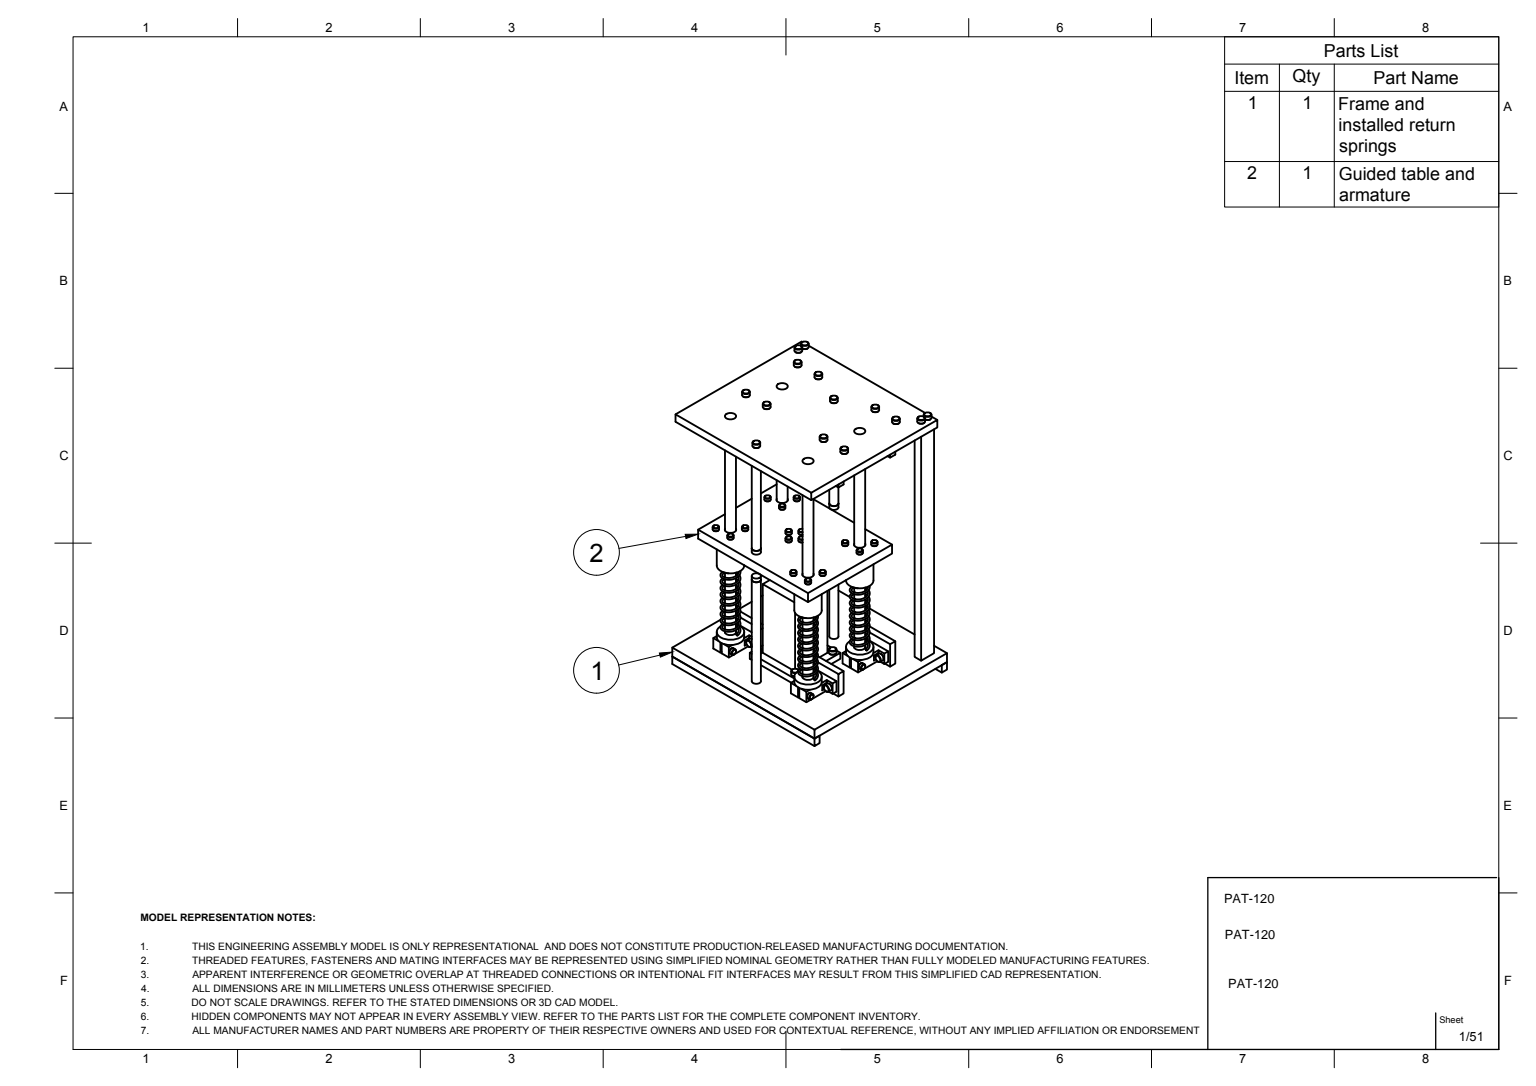
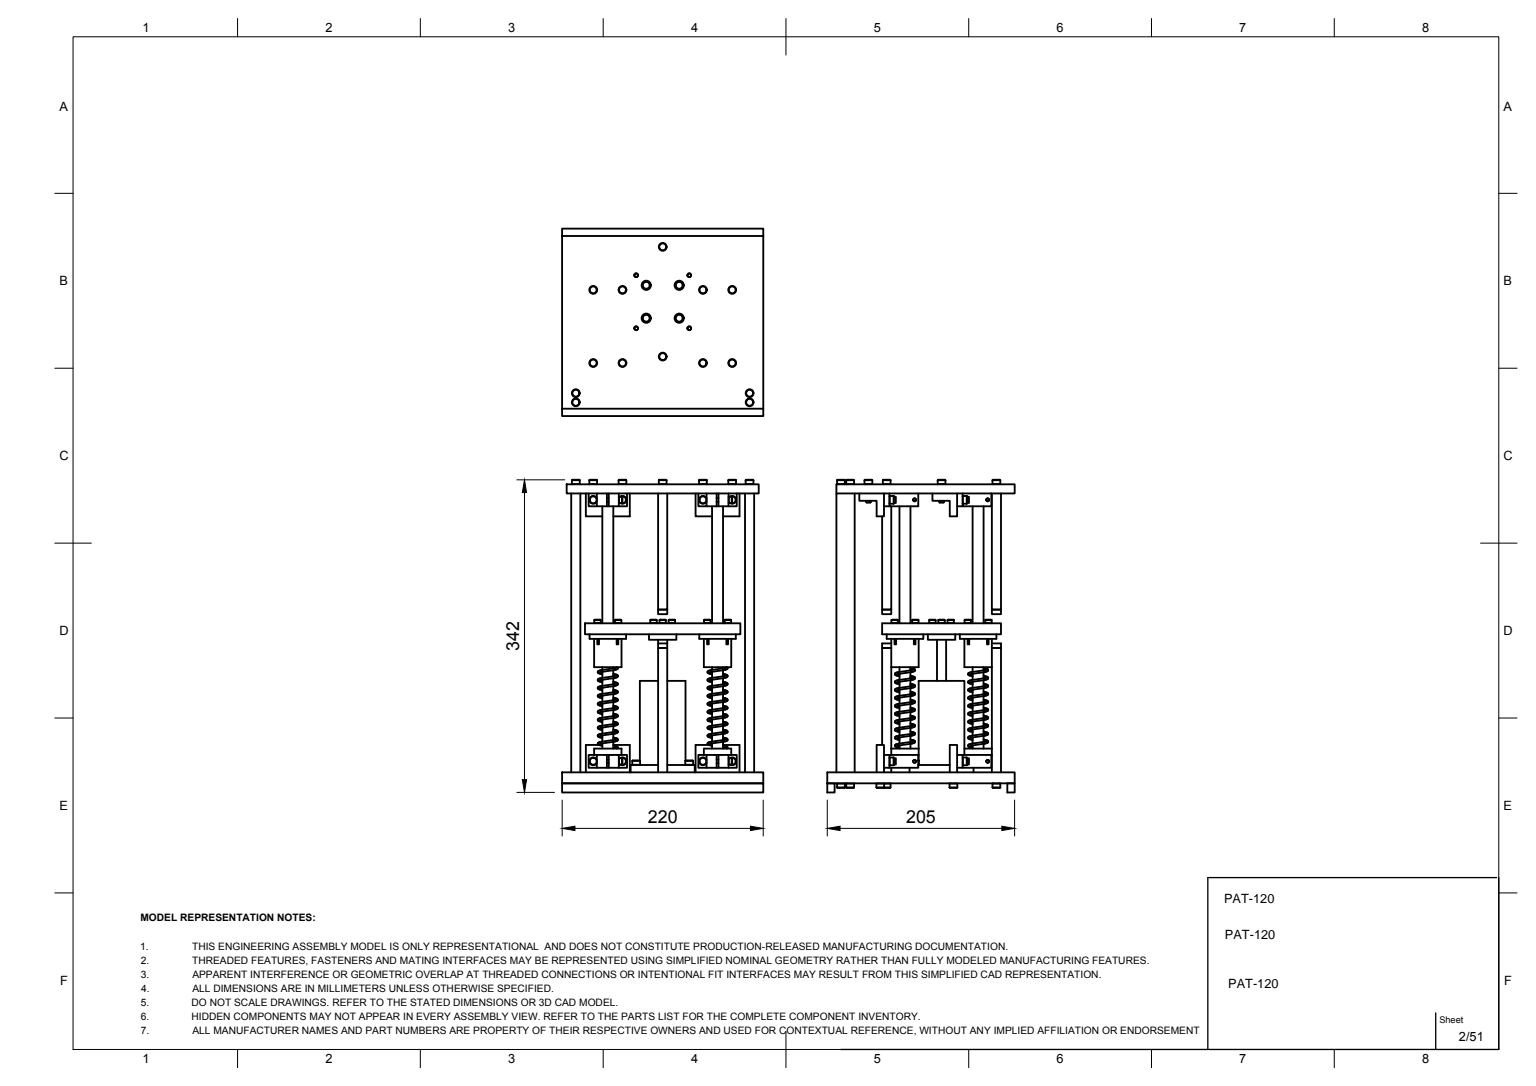
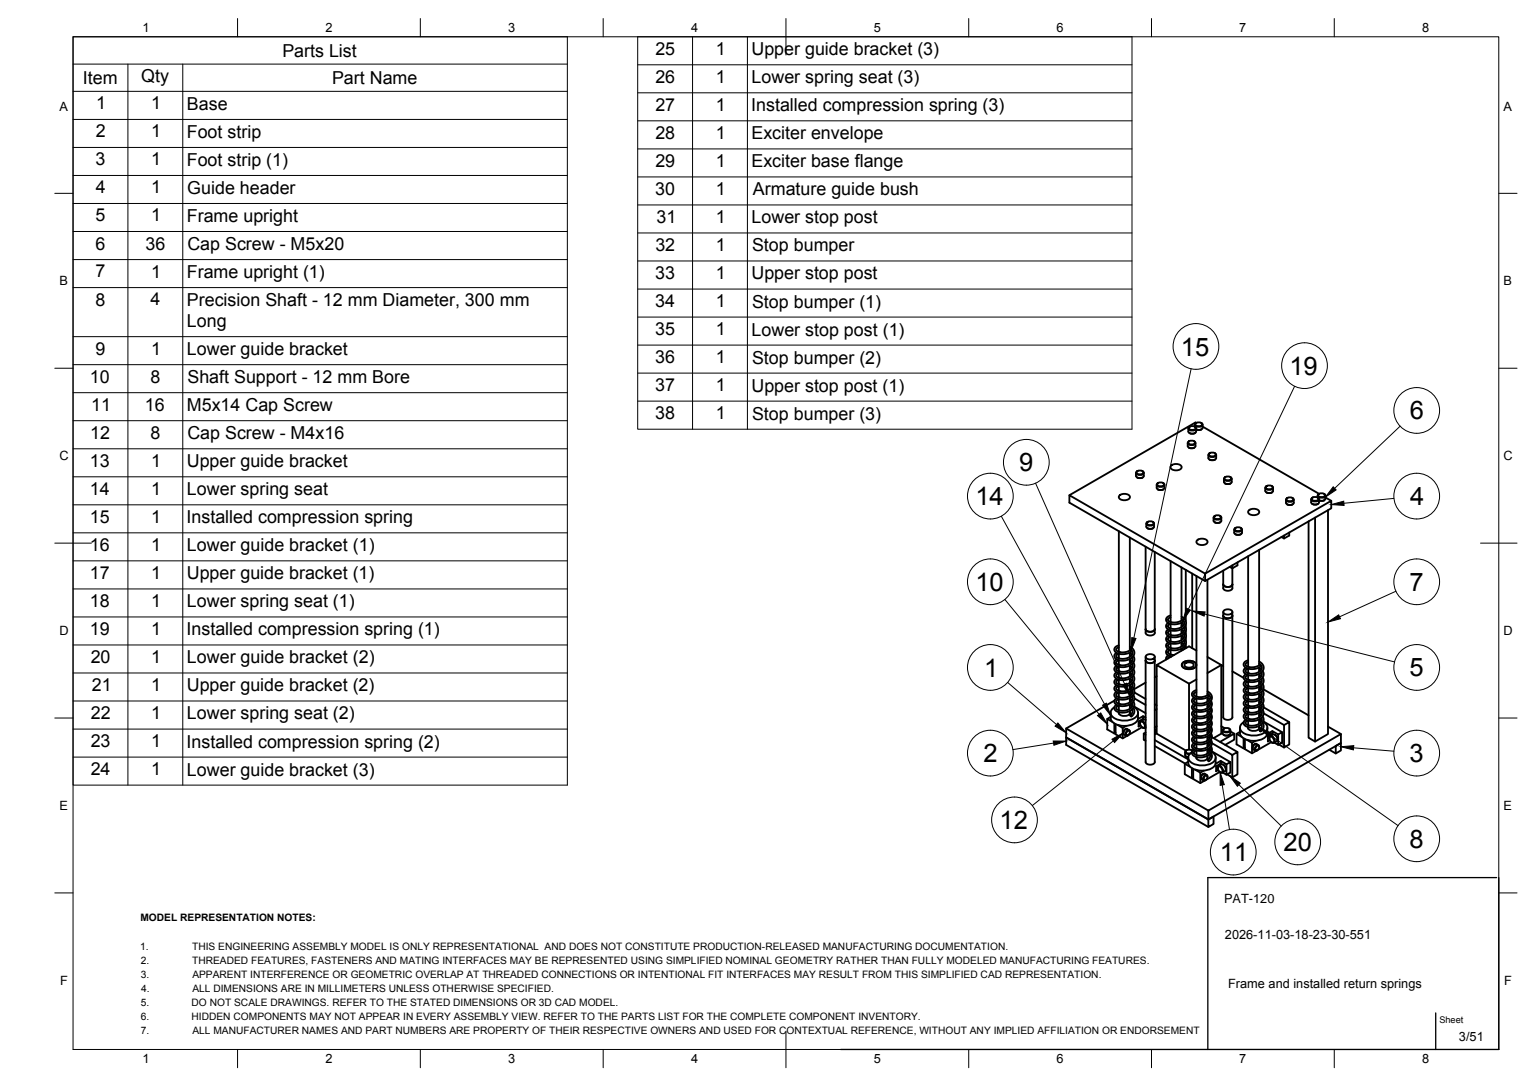
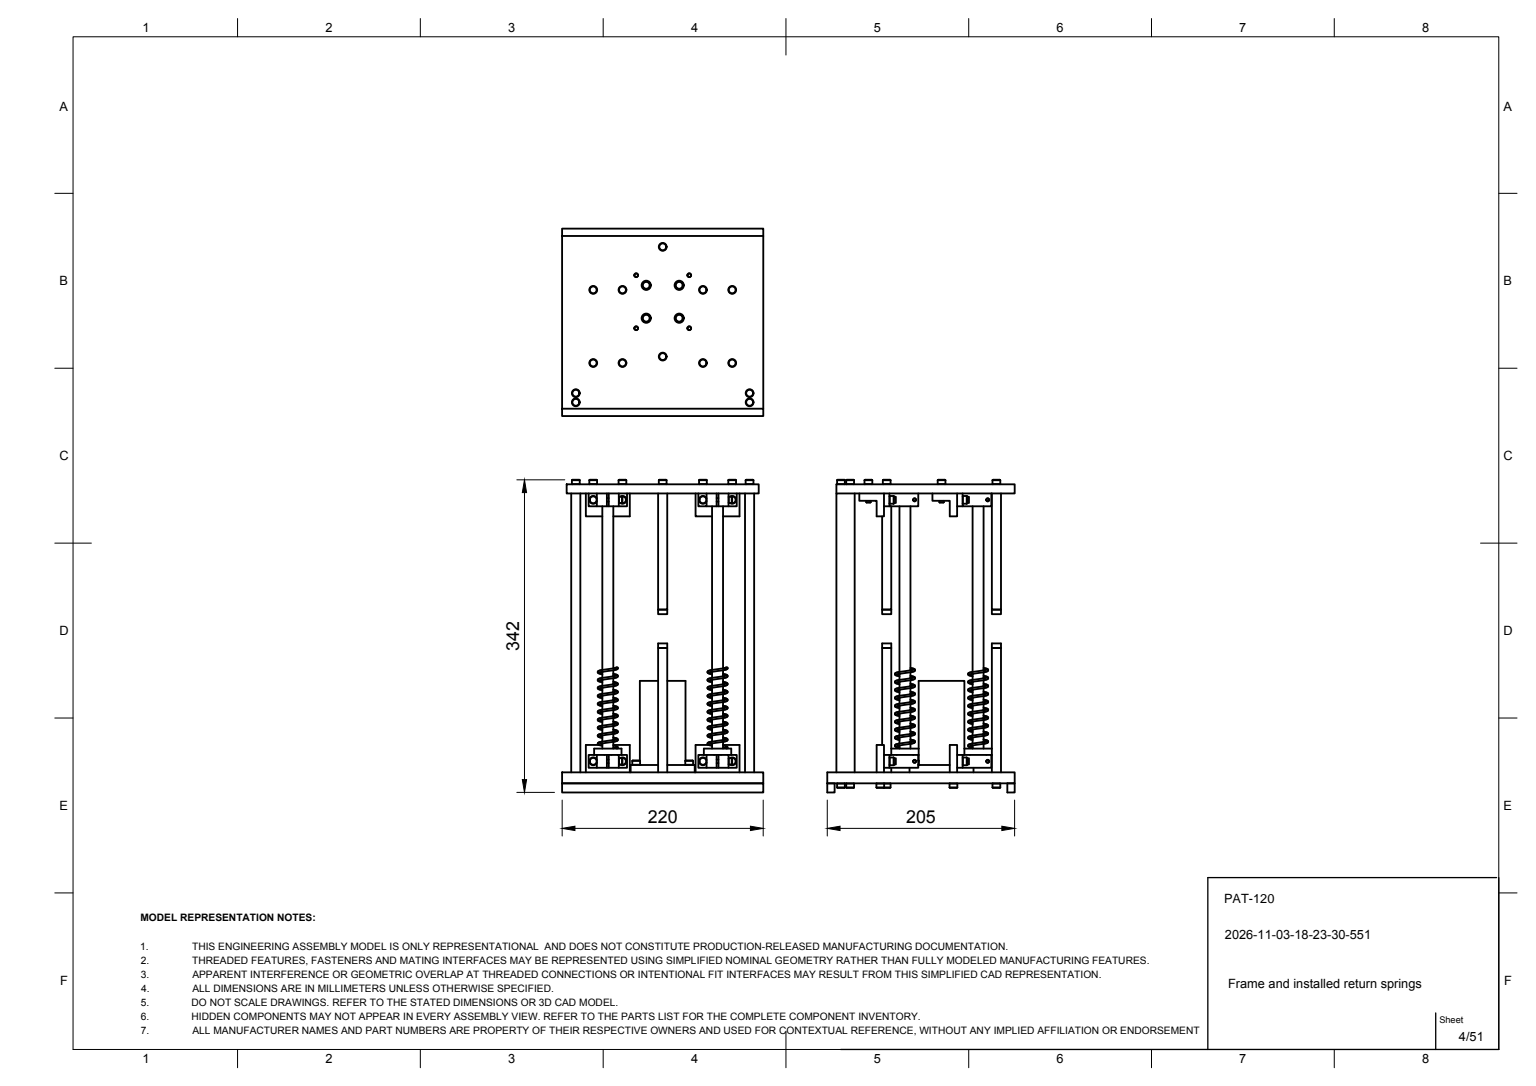
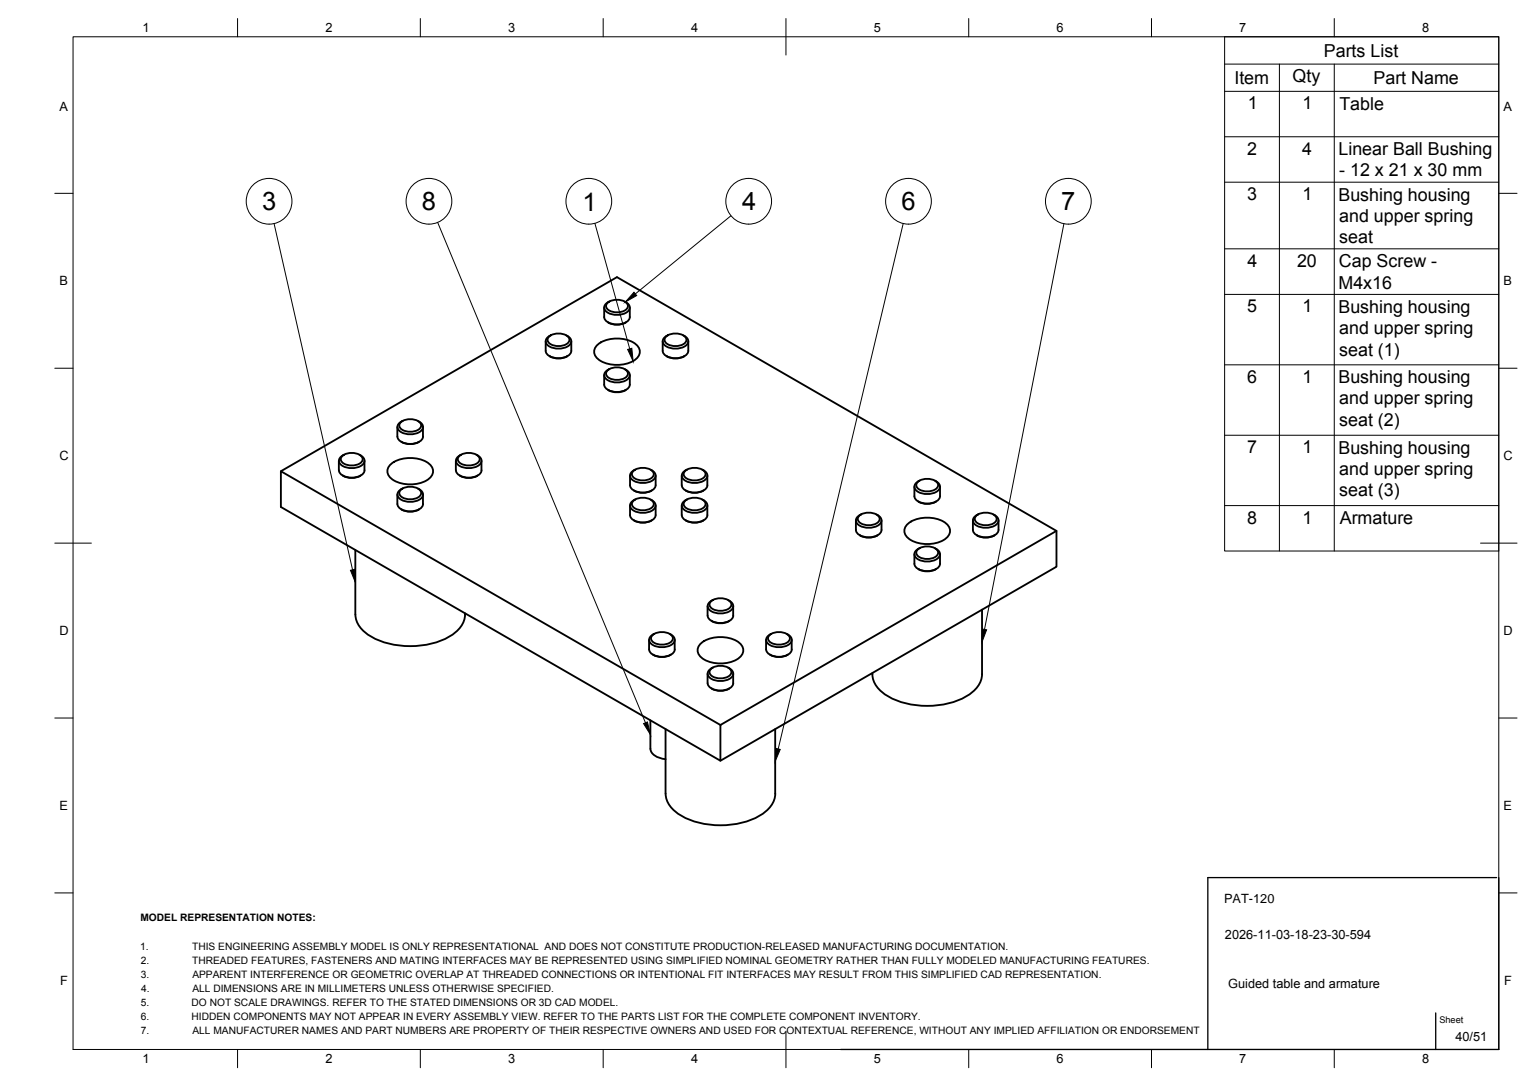
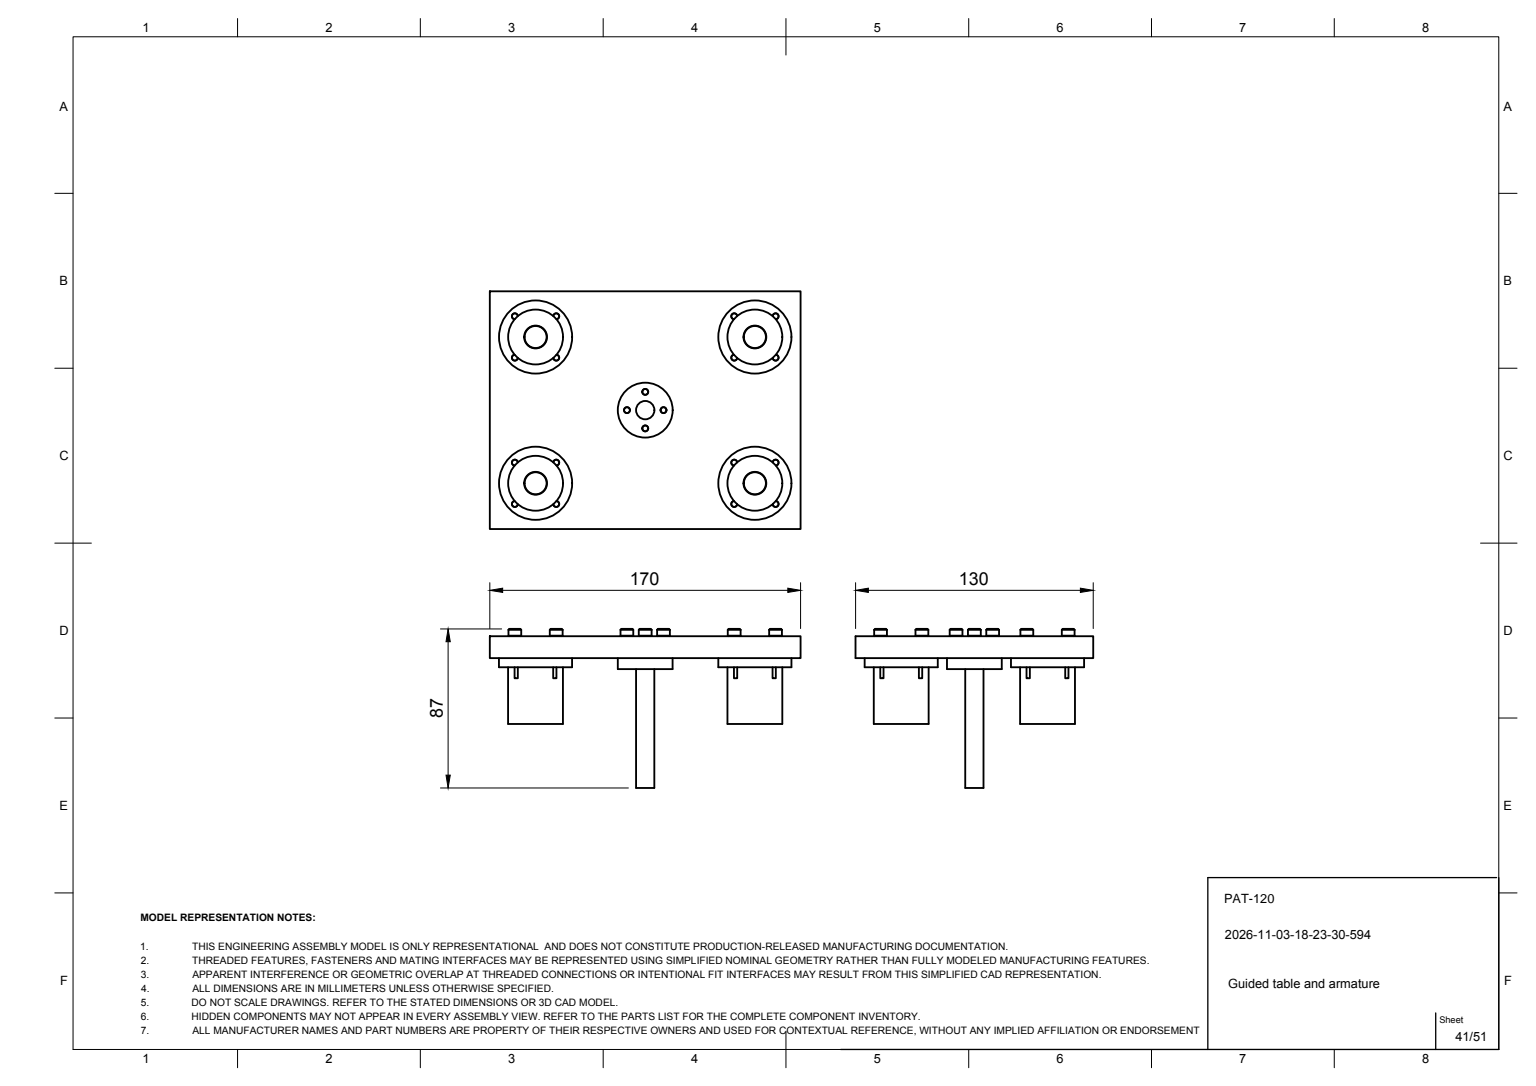
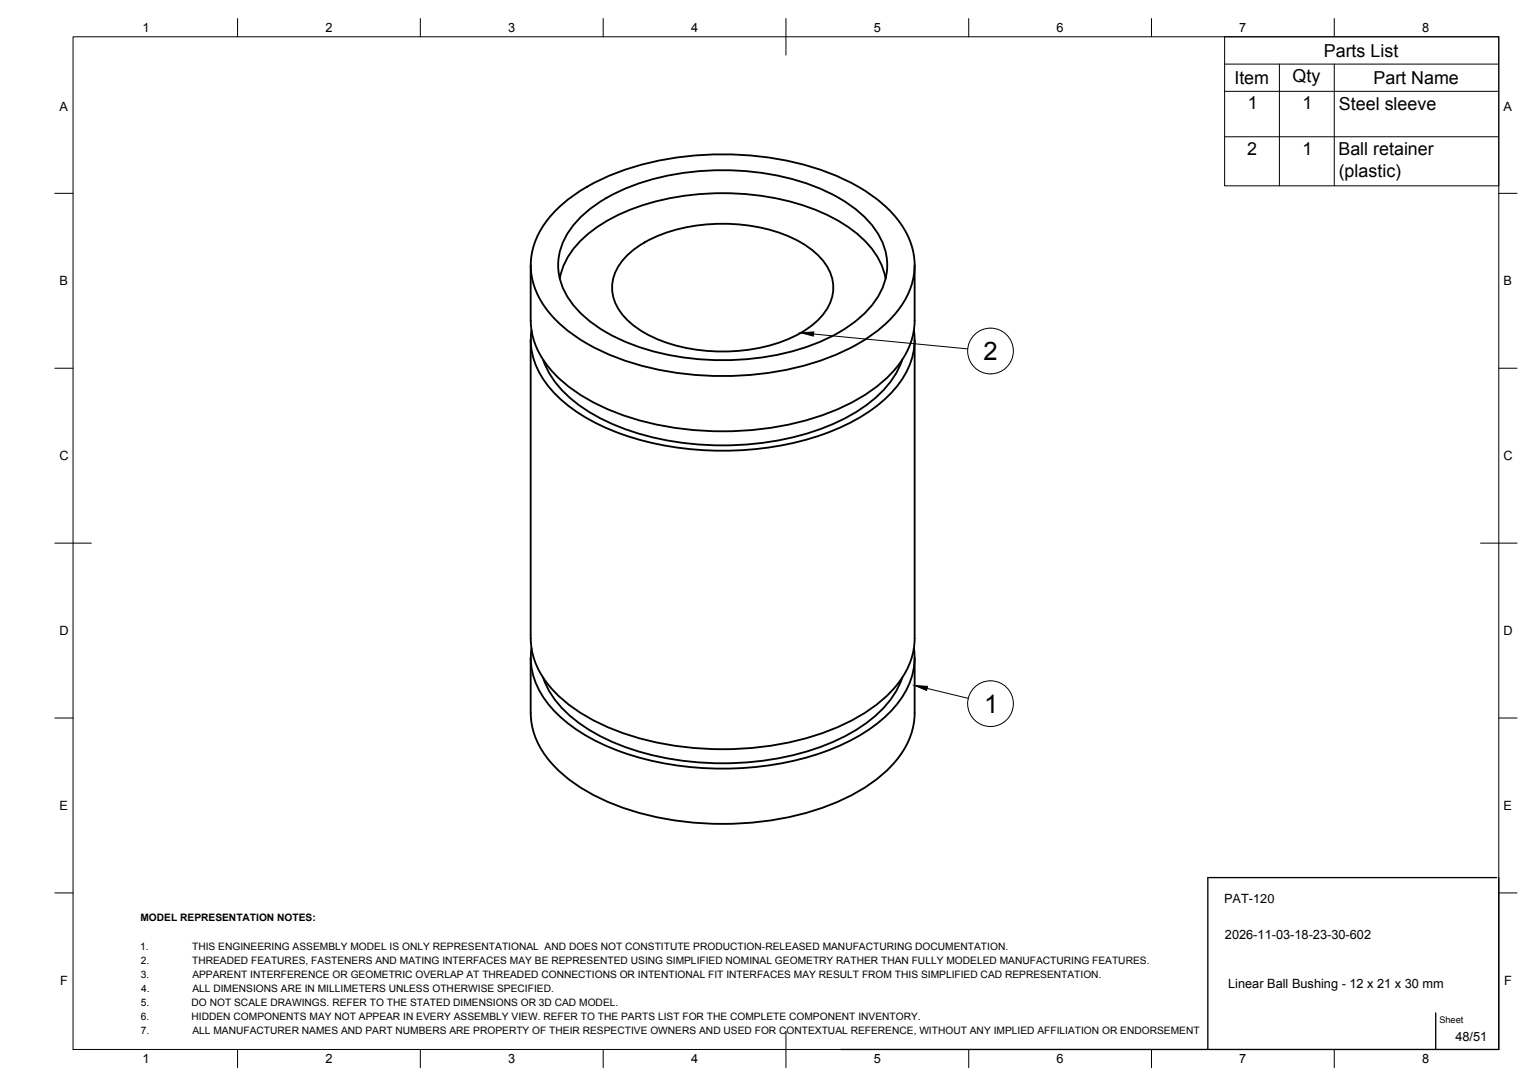
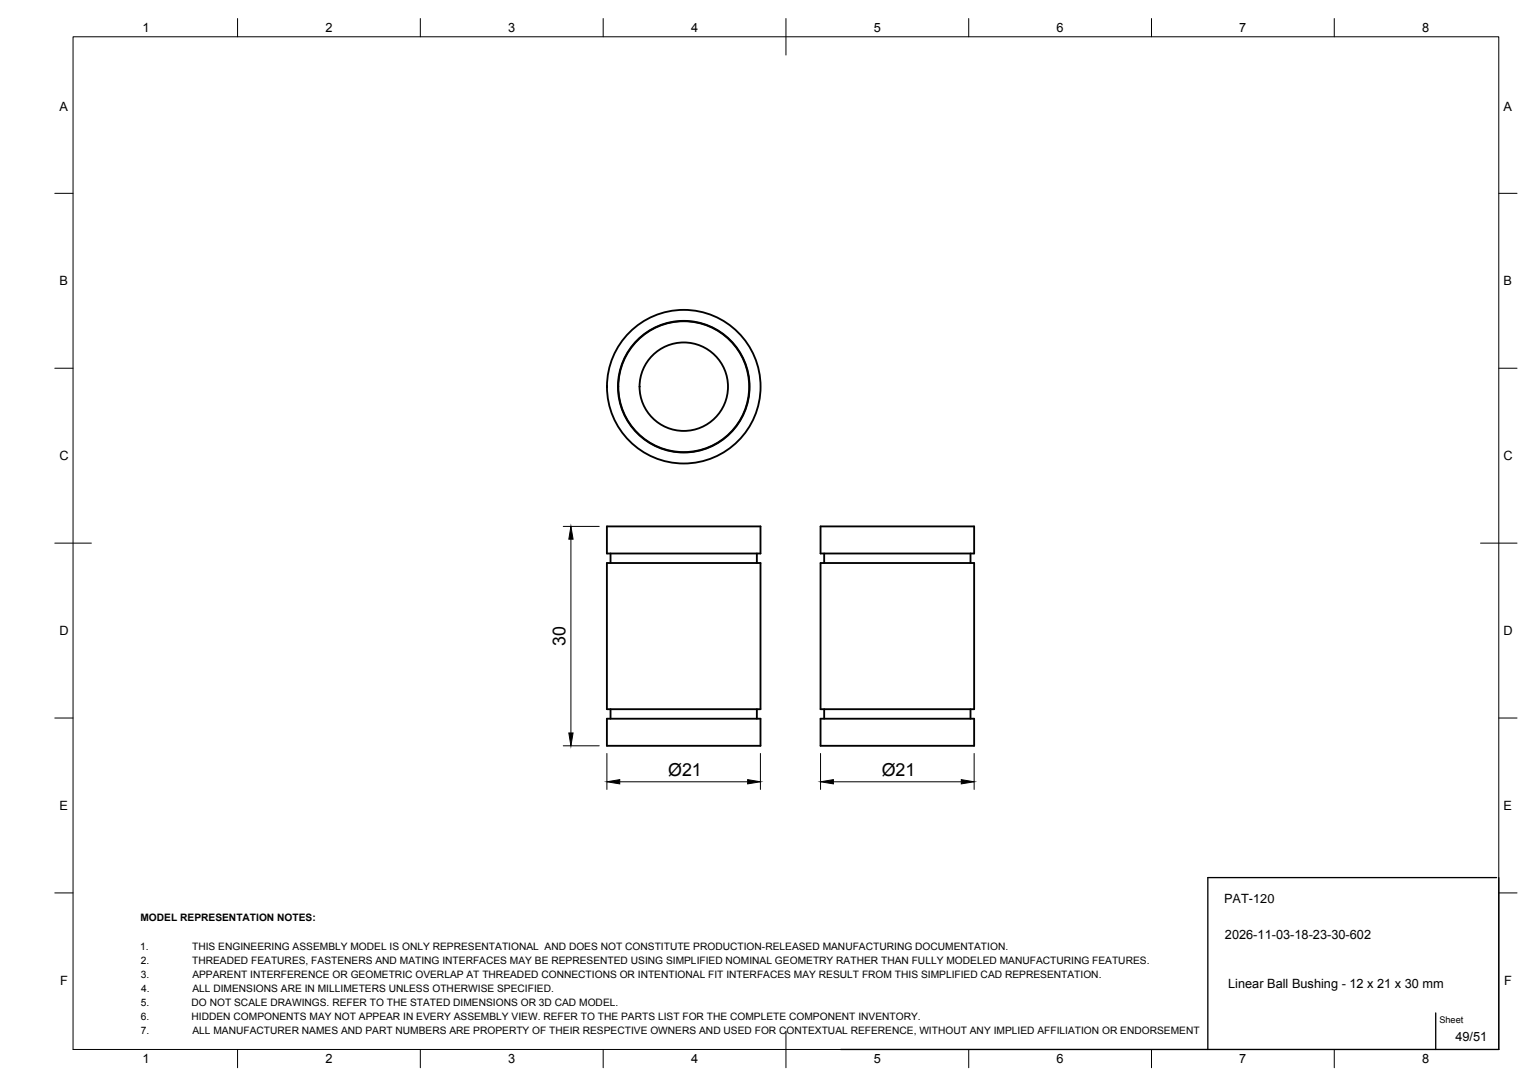
ISO-10303-21;
HEADER;
/* Generated by software containing ST-Developer
 * from STEP Tools, Inc. (www.steptools.com) 
 */

FILE_DESCRIPTION(
/* description */ ('Vibration shaker table dummy'),
/* implementation_level */ '2;1');

FILE_NAME(
/* name */ 'PAT-120',
/* time_stamp */ '2026-10-27T10:55:14-07:00',
/* author */ (''),
/* organization */ (''),
/* preprocessor_version */ 'ST-DEVELOPER v20.2',
/* originating_system */ 'Autodesk Translation Framework v15.17.0.0',
/* authorisation */ '');

FILE_SCHEMA (('AUTOMOTIVE_DESIGN { 1 0 10303 214 3 1 1 }'));
ENDSEC;

DATA;
#10=MECHANICAL_DESIGN_GEOMETRIC_PRESENTATION_REPRESENTATION('',(#686,#687,
#688,#689,#690,#691,#692,#693,#694,#695,#696,#697,#698,#699,#700,#701,#702,
#703,#704,#705,#706,#707,#708,#709,#710,#711,#712,#713,#714,#715,#716,#717,
#718,#719,#720,#721,#722,#723,#724,#725,#726,#727,#728,#729,#730,#731),
#22394);
#11=ITEM_DEFINED_TRANSFORMATION($,$,#10736,#10785);
#12=ITEM_DEFINED_TRANSFORMATION($,$,#10768,#10786);
#13=ITEM_DEFINED_TRANSFORMATION($,$,#9762,#10813);
#14=ITEM_DEFINED_TRANSFORMATION($,$,#9835,#10814);
#15=ITEM_DEFINED_TRANSFORMATION($,$,#9842,#10815);
#16=ITEM_DEFINED_TRANSFORMATION($,$,#9849,#10816);
#17=ITEM_DEFINED_TRANSFORMATION($,$,#9910,#10817);
#18=ITEM_DEFINED_TRANSFORMATION($,$,#9933,#10818);
#19=ITEM_DEFINED_TRANSFORMATION($,$,#9956,#10819);
#20=ITEM_DEFINED_TRANSFORMATION($,$,#9977,#10820);
#21=ITEM_DEFINED_TRANSFORMATION($,$,#10004,#10821);
#22=ITEM_DEFINED_TRANSFORMATION($,$,#10013,#10822);
#23=ITEM_DEFINED_TRANSFORMATION($,$,#10018,#10823);
#24=ITEM_DEFINED_TRANSFORMATION($,$,#10039,#10824);
#25=ITEM_DEFINED_TRANSFORMATION($,$,#10066,#10825);
#26=ITEM_DEFINED_TRANSFORMATION($,$,#10075,#10826);
#27=ITEM_DEFINED_TRANSFORMATION($,$,#10080,#10827);
#28=ITEM_DEFINED_TRANSFORMATION($,$,#10101,#10828);
#29=ITEM_DEFINED_TRANSFORMATION($,$,#10128,#10829);
#30=ITEM_DEFINED_TRANSFORMATION($,$,#10137,#10830);
#31=ITEM_DEFINED_TRANSFORMATION($,$,#10142,#10831);
#32=ITEM_DEFINED_TRANSFORMATION($,$,#10163,#10832);
#33=ITEM_DEFINED_TRANSFORMATION($,$,#10190,#10833);
#34=ITEM_DEFINED_TRANSFORMATION($,$,#10199,#10834);
#35=ITEM_DEFINED_TRANSFORMATION($,$,#10204,#10835);
#36=ITEM_DEFINED_TRANSFORMATION($,$,#10235,#10836);
#37=ITEM_DEFINED_TRANSFORMATION($,$,#10266,#10837);
#38=ITEM_DEFINED_TRANSFORMATION($,$,#10275,#10838);
#39=ITEM_DEFINED_TRANSFORMATION($,$,#10285,#10839);
#40=ITEM_DEFINED_TRANSFORMATION($,$,#10291,#10840);
#41=ITEM_DEFINED_TRANSFORMATION($,$,#10301,#10841);
#42=ITEM_DEFINED_TRANSFORMATION($,$,#10307,#10842);
#43=ITEM_DEFINED_TRANSFORMATION($,$,#10317,#10843);
#44=ITEM_DEFINED_TRANSFORMATION($,$,#10323,#10844);
#45=ITEM_DEFINED_TRANSFORMATION($,$,#10333,#10845);
#46=ITEM_DEFINED_TRANSFORMATION($,$,#10411,#10846);
#47=ITEM_DEFINED_TRANSFORMATION($,$,#10411,#10847);
#48=ITEM_DEFINED_TRANSFORMATION($,$,#10411,#10848);
#49=ITEM_DEFINED_TRANSFORMATION($,$,#10411,#10849);
#50=ITEM_DEFINED_TRANSFORMATION($,$,#10411,#10850);
#51=ITEM_DEFINED_TRANSFORMATION($,$,#10411,#10851);
#52=ITEM_DEFINED_TRANSFORMATION($,$,#10411,#10852);
#53=ITEM_DEFINED_TRANSFORMATION($,$,#10411,#10853);
#54=ITEM_DEFINED_TRANSFORMATION($,$,#10339,#10854);
#55=ITEM_DEFINED_TRANSFORMATION($,$,#10349,#10855);
#56=ITEM_DEFINED_TRANSFORMATION($,$,#10387,#10856);
#57=ITEM_DEFINED_TRANSFORMATION($,$,#10387,#10857);
#58=ITEM_DEFINED_TRANSFORMATION($,$,#10787,#10858);
#59=ITEM_DEFINED_TRANSFORMATION($,$,#10411,#10859);
#60=ITEM_DEFINED_TRANSFORMATION($,$,#10411,#10860);
#61=ITEM_DEFINED_TRANSFORMATION($,$,#10349,#10861);
#62=ITEM_DEFINED_TRANSFORMATION($,$,#10387,#10862);
#63=ITEM_DEFINED_TRANSFORMATION($,$,#10387,#10863);
#64=ITEM_DEFINED_TRANSFORMATION($,$,#10787,#10864);
#65=ITEM_DEFINED_TRANSFORMATION($,$,#10411,#10865);
#66=ITEM_DEFINED_TRANSFORMATION($,$,#10411,#10866);
#67=ITEM_DEFINED_TRANSFORMATION($,$,#10339,#10867);
#68=ITEM_DEFINED_TRANSFORMATION($,$,#10349,#10868);
#69=ITEM_DEFINED_TRANSFORMATION($,$,#10387,#10869);
#70=ITEM_DEFINED_TRANSFORMATION($,$,#10387,#10870);
#71=ITEM_DEFINED_TRANSFORMATION($,$,#10787,#10871);
#72=ITEM_DEFINED_TRANSFORMATION($,$,#10411,#10872);
#73=ITEM_DEFINED_TRANSFORMATION($,$,#10411,#10873);
#74=ITEM_DEFINED_TRANSFORMATION($,$,#10349,#10874);
#75=ITEM_DEFINED_TRANSFORMATION($,$,#10387,#10875);
#76=ITEM_DEFINED_TRANSFORMATION($,$,#10387,#10876);
#77=ITEM_DEFINED_TRANSFORMATION($,$,#10787,#10877);
#78=ITEM_DEFINED_TRANSFORMATION($,$,#10411,#10878);
#79=ITEM_DEFINED_TRANSFORMATION($,$,#10411,#10879);
#80=ITEM_DEFINED_TRANSFORMATION($,$,#10339,#10880);
#81=ITEM_DEFINED_TRANSFORMATION($,$,#10349,#10881);
#82=ITEM_DEFINED_TRANSFORMATION($,$,#10387,#10882);
#83=ITEM_DEFINED_TRANSFORMATION($,$,#10387,#10883);
#84=ITEM_DEFINED_TRANSFORMATION($,$,#10787,#10884);
#85=ITEM_DEFINED_TRANSFORMATION($,$,#10411,#10885);
#86=ITEM_DEFINED_TRANSFORMATION($,$,#10411,#10886);
#87=ITEM_DEFINED_TRANSFORMATION($,$,#10349,#10887);
#88=ITEM_DEFINED_TRANSFORMATION($,$,#10387,#10888);
#89=ITEM_DEFINED_TRANSFORMATION($,$,#10387,#10889);
#90=ITEM_DEFINED_TRANSFORMATION($,$,#10787,#10890);
#91=ITEM_DEFINED_TRANSFORMATION($,$,#10411,#10891);
#92=ITEM_DEFINED_TRANSFORMATION($,$,#10411,#10892);
#93=ITEM_DEFINED_TRANSFORMATION($,$,#10339,#10893);
#94=ITEM_DEFINED_TRANSFORMATION($,$,#10349,#10894);
#95=ITEM_DEFINED_TRANSFORMATION($,$,#10387,#10895);
#96=ITEM_DEFINED_TRANSFORMATION($,$,#10387,#10896);
#97=ITEM_DEFINED_TRANSFORMATION($,$,#10787,#10897);
#98=ITEM_DEFINED_TRANSFORMATION($,$,#10411,#10898);
#99=ITEM_DEFINED_TRANSFORMATION($,$,#10411,#10899);
#100=ITEM_DEFINED_TRANSFORMATION($,$,#10349,#10900);
#101=ITEM_DEFINED_TRANSFORMATION($,$,#10387,#10901);
#102=ITEM_DEFINED_TRANSFORMATION($,$,#10387,#10902);
#103=ITEM_DEFINED_TRANSFORMATION($,$,#10787,#10903);
#104=ITEM_DEFINED_TRANSFORMATION($,$,#10411,#10904);
#105=ITEM_DEFINED_TRANSFORMATION($,$,#10411,#10905);
#106=ITEM_DEFINED_TRANSFORMATION($,$,#10411,#10906);
#107=ITEM_DEFINED_TRANSFORMATION($,$,#10411,#10907);
#108=ITEM_DEFINED_TRANSFORMATION($,$,#10411,#10908);
#109=ITEM_DEFINED_TRANSFORMATION($,$,#10411,#10909);
#110=ITEM_DEFINED_TRANSFORMATION($,$,#10411,#10910);
#111=ITEM_DEFINED_TRANSFORMATION($,$,#10411,#10911);
#112=ITEM_DEFINED_TRANSFORMATION($,$,#10411,#10912);
#113=ITEM_DEFINED_TRANSFORMATION($,$,#10411,#10913);
#114=ITEM_DEFINED_TRANSFORMATION($,$,#10411,#10914);
#115=ITEM_DEFINED_TRANSFORMATION($,$,#10411,#10915);
#116=ITEM_DEFINED_TRANSFORMATION($,$,#10411,#10916);
#117=ITEM_DEFINED_TRANSFORMATION($,$,#10411,#10917);
#118=ITEM_DEFINED_TRANSFORMATION($,$,#10438,#10918);
#119=ITEM_DEFINED_TRANSFORMATION($,$,#10517,#10919);
#120=ITEM_DEFINED_TRANSFORMATION($,$,#10566,#10920);
#121=ITEM_DEFINED_TRANSFORMATION($,$,#10615,#10921);
#122=ITEM_DEFINED_TRANSFORMATION($,$,#10664,#10922);
#123=ITEM_DEFINED_TRANSFORMATION($,$,#10713,#10923);
#124=ITEM_DEFINED_TRANSFORMATION($,$,#10735,#10924);
#125=ITEM_DEFINED_TRANSFORMATION($,$,#10787,#10925);
#126=ITEM_DEFINED_TRANSFORMATION($,$,#10787,#10926);
#127=ITEM_DEFINED_TRANSFORMATION($,$,#10787,#10927);
#128=ITEM_DEFINED_TRANSFORMATION($,$,#10787,#10928);
#129=ITEM_DEFINED_TRANSFORMATION($,$,#10735,#10929);
#130=ITEM_DEFINED_TRANSFORMATION($,$,#10787,#10930);
#131=ITEM_DEFINED_TRANSFORMATION($,$,#10787,#10931);
#132=ITEM_DEFINED_TRANSFORMATION($,$,#10787,#10932);
#133=ITEM_DEFINED_TRANSFORMATION($,$,#10787,#10933);
#134=ITEM_DEFINED_TRANSFORMATION($,$,#10735,#10934);
#135=ITEM_DEFINED_TRANSFORMATION($,$,#10787,#10935);
#136=ITEM_DEFINED_TRANSFORMATION($,$,#10787,#10936);
#137=ITEM_DEFINED_TRANSFORMATION($,$,#10787,#10937);
#138=ITEM_DEFINED_TRANSFORMATION($,$,#10787,#10938);
#139=ITEM_DEFINED_TRANSFORMATION($,$,#10735,#10939);
#140=ITEM_DEFINED_TRANSFORMATION($,$,#10787,#10940);
#141=ITEM_DEFINED_TRANSFORMATION($,$,#10787,#10941);
#142=ITEM_DEFINED_TRANSFORMATION($,$,#10787,#10942);
#143=ITEM_DEFINED_TRANSFORMATION($,$,#10787,#10943);
#144=ITEM_DEFINED_TRANSFORMATION($,$,#10787,#10944);
#145=ITEM_DEFINED_TRANSFORMATION($,$,#10787,#10945);
#146=ITEM_DEFINED_TRANSFORMATION($,$,#10787,#10946);
#147=ITEM_DEFINED_TRANSFORMATION($,$,#10787,#10947);
#148=ITEM_DEFINED_TRANSFORMATION($,$,#9761,#10948);
#149=ITEM_DEFINED_TRANSFORMATION($,$,#10437,#10949);
#150=(
REPRESENTATION_RELATIONSHIP($,$,#22685,#22684)
REPRESENTATION_RELATIONSHIP_WITH_TRANSFORMATION(#11)
SHAPE_REPRESENTATION_RELATIONSHIP()
);
#151=(
REPRESENTATION_RELATIONSHIP($,$,#22686,#22684)
REPRESENTATION_RELATIONSHIP_WITH_TRANSFORMATION(#12)
SHAPE_REPRESENTATION_RELATIONSHIP()
);
#152=(
REPRESENTATION_RELATIONSHIP($,$,#22640,#22639)
REPRESENTATION_RELATIONSHIP_WITH_TRANSFORMATION(#13)
SHAPE_REPRESENTATION_RELATIONSHIP()
);
#153=(
REPRESENTATION_RELATIONSHIP($,$,#22641,#22639)
REPRESENTATION_RELATIONSHIP_WITH_TRANSFORMATION(#14)
SHAPE_REPRESENTATION_RELATIONSHIP()
);
#154=(
REPRESENTATION_RELATIONSHIP($,$,#22642,#22639)
REPRESENTATION_RELATIONSHIP_WITH_TRANSFORMATION(#15)
SHAPE_REPRESENTATION_RELATIONSHIP()
);
#155=(
REPRESENTATION_RELATIONSHIP($,$,#22643,#22639)
REPRESENTATION_RELATIONSHIP_WITH_TRANSFORMATION(#16)
SHAPE_REPRESENTATION_RELATIONSHIP()
);
#156=(
REPRESENTATION_RELATIONSHIP($,$,#22644,#22639)
REPRESENTATION_RELATIONSHIP_WITH_TRANSFORMATION(#17)
SHAPE_REPRESENTATION_RELATIONSHIP()
);
#157=(
REPRESENTATION_RELATIONSHIP($,$,#22645,#22639)
REPRESENTATION_RELATIONSHIP_WITH_TRANSFORMATION(#18)
SHAPE_REPRESENTATION_RELATIONSHIP()
);
#158=(
REPRESENTATION_RELATIONSHIP($,$,#22646,#22639)
REPRESENTATION_RELATIONSHIP_WITH_TRANSFORMATION(#19)
SHAPE_REPRESENTATION_RELATIONSHIP()
);
#159=(
REPRESENTATION_RELATIONSHIP($,$,#22647,#22639)
REPRESENTATION_RELATIONSHIP_WITH_TRANSFORMATION(#20)
SHAPE_REPRESENTATION_RELATIONSHIP()
);
#160=(
REPRESENTATION_RELATIONSHIP($,$,#22648,#22639)
REPRESENTATION_RELATIONSHIP_WITH_TRANSFORMATION(#21)
SHAPE_REPRESENTATION_RELATIONSHIP()
);
#161=(
REPRESENTATION_RELATIONSHIP($,$,#22649,#22639)
REPRESENTATION_RELATIONSHIP_WITH_TRANSFORMATION(#22)
SHAPE_REPRESENTATION_RELATIONSHIP()
);
#162=(
REPRESENTATION_RELATIONSHIP($,$,#22650,#22639)
REPRESENTATION_RELATIONSHIP_WITH_TRANSFORMATION(#23)
SHAPE_REPRESENTATION_RELATIONSHIP()
);
#163=(
REPRESENTATION_RELATIONSHIP($,$,#22651,#22639)
REPRESENTATION_RELATIONSHIP_WITH_TRANSFORMATION(#24)
SHAPE_REPRESENTATION_RELATIONSHIP()
);
#164=(
REPRESENTATION_RELATIONSHIP($,$,#22652,#22639)
REPRESENTATION_RELATIONSHIP_WITH_TRANSFORMATION(#25)
SHAPE_REPRESENTATION_RELATIONSHIP()
);
#165=(
REPRESENTATION_RELATIONSHIP($,$,#22653,#22639)
REPRESENTATION_RELATIONSHIP_WITH_TRANSFORMATION(#26)
SHAPE_REPRESENTATION_RELATIONSHIP()
);
#166=(
REPRESENTATION_RELATIONSHIP($,$,#22654,#22639)
REPRESENTATION_RELATIONSHIP_WITH_TRANSFORMATION(#27)
SHAPE_REPRESENTATION_RELATIONSHIP()
);
#167=(
REPRESENTATION_RELATIONSHIP($,$,#22655,#22639)
REPRESENTATION_RELATIONSHIP_WITH_TRANSFORMATION(#28)
SHAPE_REPRESENTATION_RELATIONSHIP()
);
#168=(
REPRESENTATION_RELATIONSHIP($,$,#22656,#22639)
REPRESENTATION_RELATIONSHIP_WITH_TRANSFORMATION(#29)
SHAPE_REPRESENTATION_RELATIONSHIP()
);
#169=(
REPRESENTATION_RELATIONSHIP($,$,#22657,#22639)
REPRESENTATION_RELATIONSHIP_WITH_TRANSFORMATION(#30)
SHAPE_REPRESENTATION_RELATIONSHIP()
);
#170=(
REPRESENTATION_RELATIONSHIP($,$,#22658,#22639)
REPRESENTATION_RELATIONSHIP_WITH_TRANSFORMATION(#31)
SHAPE_REPRESENTATION_RELATIONSHIP()
);
#171=(
REPRESENTATION_RELATIONSHIP($,$,#22659,#22639)
REPRESENTATION_RELATIONSHIP_WITH_TRANSFORMATION(#32)
SHAPE_REPRESENTATION_RELATIONSHIP()
);
#172=(
REPRESENTATION_RELATIONSHIP($,$,#22660,#22639)
REPRESENTATION_RELATIONSHIP_WITH_TRANSFORMATION(#33)
SHAPE_REPRESENTATION_RELATIONSHIP()
);
#173=(
REPRESENTATION_RELATIONSHIP($,$,#22661,#22639)
REPRESENTATION_RELATIONSHIP_WITH_TRANSFORMATION(#34)
SHAPE_REPRESENTATION_RELATIONSHIP()
);
#174=(
REPRESENTATION_RELATIONSHIP($,$,#22662,#22639)
REPRESENTATION_RELATIONSHIP_WITH_TRANSFORMATION(#35)
SHAPE_REPRESENTATION_RELATIONSHIP()
);
#175=(
REPRESENTATION_RELATIONSHIP($,$,#22663,#22639)
REPRESENTATION_RELATIONSHIP_WITH_TRANSFORMATION(#36)
SHAPE_REPRESENTATION_RELATIONSHIP()
);
#176=(
REPRESENTATION_RELATIONSHIP($,$,#22664,#22639)
REPRESENTATION_RELATIONSHIP_WITH_TRANSFORMATION(#37)
SHAPE_REPRESENTATION_RELATIONSHIP()
);
#177=(
REPRESENTATION_RELATIONSHIP($,$,#22665,#22639)
REPRESENTATION_RELATIONSHIP_WITH_TRANSFORMATION(#38)
SHAPE_REPRESENTATION_RELATIONSHIP()
);
#178=(
REPRESENTATION_RELATIONSHIP($,$,#22666,#22639)
REPRESENTATION_RELATIONSHIP_WITH_TRANSFORMATION(#39)
SHAPE_REPRESENTATION_RELATIONSHIP()
);
#179=(
REPRESENTATION_RELATIONSHIP($,$,#22667,#22639)
REPRESENTATION_RELATIONSHIP_WITH_TRANSFORMATION(#40)
SHAPE_REPRESENTATION_RELATIONSHIP()
);
#180=(
REPRESENTATION_RELATIONSHIP($,$,#22668,#22639)
REPRESENTATION_RELATIONSHIP_WITH_TRANSFORMATION(#41)
SHAPE_REPRESENTATION_RELATIONSHIP()
);
#181=(
REPRESENTATION_RELATIONSHIP($,$,#22669,#22639)
REPRESENTATION_RELATIONSHIP_WITH_TRANSFORMATION(#42)
SHAPE_REPRESENTATION_RELATIONSHIP()
);
#182=(
REPRESENTATION_RELATIONSHIP($,$,#22670,#22639)
REPRESENTATION_RELATIONSHIP_WITH_TRANSFORMATION(#43)
SHAPE_REPRESENTATION_RELATIONSHIP()
);
#183=(
REPRESENTATION_RELATIONSHIP($,$,#22671,#22639)
REPRESENTATION_RELATIONSHIP_WITH_TRANSFORMATION(#44)
SHAPE_REPRESENTATION_RELATIONSHIP()
);
#184=(
REPRESENTATION_RELATIONSHIP($,$,#22672,#22639)
REPRESENTATION_RELATIONSHIP_WITH_TRANSFORMATION(#45)
SHAPE_REPRESENTATION_RELATIONSHIP()
);
#185=(
REPRESENTATION_RELATIONSHIP($,$,#22676,#22639)
REPRESENTATION_RELATIONSHIP_WITH_TRANSFORMATION(#46)
SHAPE_REPRESENTATION_RELATIONSHIP()
);
#186=(
REPRESENTATION_RELATIONSHIP($,$,#22676,#22639)
REPRESENTATION_RELATIONSHIP_WITH_TRANSFORMATION(#47)
SHAPE_REPRESENTATION_RELATIONSHIP()
);
#187=(
REPRESENTATION_RELATIONSHIP($,$,#22676,#22639)
REPRESENTATION_RELATIONSHIP_WITH_TRANSFORMATION(#48)
SHAPE_REPRESENTATION_RELATIONSHIP()
);
#188=(
REPRESENTATION_RELATIONSHIP($,$,#22676,#22639)
REPRESENTATION_RELATIONSHIP_WITH_TRANSFORMATION(#49)
SHAPE_REPRESENTATION_RELATIONSHIP()
);
#189=(
REPRESENTATION_RELATIONSHIP($,$,#22676,#22639)
REPRESENTATION_RELATIONSHIP_WITH_TRANSFORMATION(#50)
SHAPE_REPRESENTATION_RELATIONSHIP()
);
#190=(
REPRESENTATION_RELATIONSHIP($,$,#22676,#22639)
REPRESENTATION_RELATIONSHIP_WITH_TRANSFORMATION(#51)
SHAPE_REPRESENTATION_RELATIONSHIP()
);
#191=(
REPRESENTATION_RELATIONSHIP($,$,#22676,#22639)
REPRESENTATION_RELATIONSHIP_WITH_TRANSFORMATION(#52)
SHAPE_REPRESENTATION_RELATIONSHIP()
);
#192=(
REPRESENTATION_RELATIONSHIP($,$,#22676,#22639)
REPRESENTATION_RELATIONSHIP_WITH_TRANSFORMATION(#53)
SHAPE_REPRESENTATION_RELATIONSHIP()
);
#193=(
REPRESENTATION_RELATIONSHIP($,$,#22673,#22639)
REPRESENTATION_RELATIONSHIP_WITH_TRANSFORMATION(#54)
SHAPE_REPRESENTATION_RELATIONSHIP()
);
#194=(
REPRESENTATION_RELATIONSHIP($,$,#22674,#22639)
REPRESENTATION_RELATIONSHIP_WITH_TRANSFORMATION(#55)
SHAPE_REPRESENTATION_RELATIONSHIP()
);
#195=(
REPRESENTATION_RELATIONSHIP($,$,#22675,#22639)
REPRESENTATION_RELATIONSHIP_WITH_TRANSFORMATION(#56)
SHAPE_REPRESENTATION_RELATIONSHIP()
);
#196=(
REPRESENTATION_RELATIONSHIP($,$,#22675,#22639)
REPRESENTATION_RELATIONSHIP_WITH_TRANSFORMATION(#57)
SHAPE_REPRESENTATION_RELATIONSHIP()
);
#197=(
REPRESENTATION_RELATIONSHIP($,$,#22687,#22639)
REPRESENTATION_RELATIONSHIP_WITH_TRANSFORMATION(#58)
SHAPE_REPRESENTATION_RELATIONSHIP()
);
#198=(
REPRESENTATION_RELATIONSHIP($,$,#22676,#22639)
REPRESENTATION_RELATIONSHIP_WITH_TRANSFORMATION(#59)
SHAPE_REPRESENTATION_RELATIONSHIP()
);
#199=(
REPRESENTATION_RELATIONSHIP($,$,#22676,#22639)
REPRESENTATION_RELATIONSHIP_WITH_TRANSFORMATION(#60)
SHAPE_REPRESENTATION_RELATIONSHIP()
);
#200=(
REPRESENTATION_RELATIONSHIP($,$,#22674,#22639)
REPRESENTATION_RELATIONSHIP_WITH_TRANSFORMATION(#61)
SHAPE_REPRESENTATION_RELATIONSHIP()
);
#201=(
REPRESENTATION_RELATIONSHIP($,$,#22675,#22639)
REPRESENTATION_RELATIONSHIP_WITH_TRANSFORMATION(#62)
SHAPE_REPRESENTATION_RELATIONSHIP()
);
#202=(
REPRESENTATION_RELATIONSHIP($,$,#22675,#22639)
REPRESENTATION_RELATIONSHIP_WITH_TRANSFORMATION(#63)
SHAPE_REPRESENTATION_RELATIONSHIP()
);
#203=(
REPRESENTATION_RELATIONSHIP($,$,#22687,#22639)
REPRESENTATION_RELATIONSHIP_WITH_TRANSFORMATION(#64)
SHAPE_REPRESENTATION_RELATIONSHIP()
);
#204=(
REPRESENTATION_RELATIONSHIP($,$,#22676,#22639)
REPRESENTATION_RELATIONSHIP_WITH_TRANSFORMATION(#65)
SHAPE_REPRESENTATION_RELATIONSHIP()
);
#205=(
REPRESENTATION_RELATIONSHIP($,$,#22676,#22639)
REPRESENTATION_RELATIONSHIP_WITH_TRANSFORMATION(#66)
SHAPE_REPRESENTATION_RELATIONSHIP()
);
#206=(
REPRESENTATION_RELATIONSHIP($,$,#22673,#22639)
REPRESENTATION_RELATIONSHIP_WITH_TRANSFORMATION(#67)
SHAPE_REPRESENTATION_RELATIONSHIP()
);
#207=(
REPRESENTATION_RELATIONSHIP($,$,#22674,#22639)
REPRESENTATION_RELATIONSHIP_WITH_TRANSFORMATION(#68)
SHAPE_REPRESENTATION_RELATIONSHIP()
);
#208=(
REPRESENTATION_RELATIONSHIP($,$,#22675,#22639)
REPRESENTATION_RELATIONSHIP_WITH_TRANSFORMATION(#69)
SHAPE_REPRESENTATION_RELATIONSHIP()
);
#209=(
REPRESENTATION_RELATIONSHIP($,$,#22675,#22639)
REPRESENTATION_RELATIONSHIP_WITH_TRANSFORMATION(#70)
SHAPE_REPRESENTATION_RELATIONSHIP()
);
#210=(
REPRESENTATION_RELATIONSHIP($,$,#22687,#22639)
REPRESENTATION_RELATIONSHIP_WITH_TRANSFORMATION(#71)
SHAPE_REPRESENTATION_RELATIONSHIP()
);
#211=(
REPRESENTATION_RELATIONSHIP($,$,#22676,#22639)
REPRESENTATION_RELATIONSHIP_WITH_TRANSFORMATION(#72)
SHAPE_REPRESENTATION_RELATIONSHIP()
);
#212=(
REPRESENTATION_RELATIONSHIP($,$,#22676,#22639)
REPRESENTATION_RELATIONSHIP_WITH_TRANSFORMATION(#73)
SHAPE_REPRESENTATION_RELATIONSHIP()
);
#213=(
REPRESENTATION_RELATIONSHIP($,$,#22674,#22639)
REPRESENTATION_RELATIONSHIP_WITH_TRANSFORMATION(#74)
SHAPE_REPRESENTATION_RELATIONSHIP()
);
#214=(
REPRESENTATION_RELATIONSHIP($,$,#22675,#22639)
REPRESENTATION_RELATIONSHIP_WITH_TRANSFORMATION(#75)
SHAPE_REPRESENTATION_RELATIONSHIP()
);
#215=(
REPRESENTATION_RELATIONSHIP($,$,#22675,#22639)
REPRESENTATION_RELATIONSHIP_WITH_TRANSFORMATION(#76)
SHAPE_REPRESENTATION_RELATIONSHIP()
);
#216=(
REPRESENTATION_RELATIONSHIP($,$,#22687,#22639)
REPRESENTATION_RELATIONSHIP_WITH_TRANSFORMATION(#77)
SHAPE_REPRESENTATION_RELATIONSHIP()
);
#217=(
REPRESENTATION_RELATIONSHIP($,$,#22676,#22639)
REPRESENTATION_RELATIONSHIP_WITH_TRANSFORMATION(#78)
SHAPE_REPRESENTATION_RELATIONSHIP()
);
#218=(
REPRESENTATION_RELATIONSHIP($,$,#22676,#22639)
REPRESENTATION_RELATIONSHIP_WITH_TRANSFORMATION(#79)
SHAPE_REPRESENTATION_RELATIONSHIP()
);
#219=(
REPRESENTATION_RELATIONSHIP($,$,#22673,#22639)
REPRESENTATION_RELATIONSHIP_WITH_TRANSFORMATION(#80)
SHAPE_REPRESENTATION_RELATIONSHIP()
);
#220=(
REPRESENTATION_RELATIONSHIP($,$,#22674,#22639)
REPRESENTATION_RELATIONSHIP_WITH_TRANSFORMATION(#81)
SHAPE_REPRESENTATION_RELATIONSHIP()
);
#221=(
REPRESENTATION_RELATIONSHIP($,$,#22675,#22639)
REPRESENTATION_RELATIONSHIP_WITH_TRANSFORMATION(#82)
SHAPE_REPRESENTATION_RELATIONSHIP()
);
#222=(
REPRESENTATION_RELATIONSHIP($,$,#22675,#22639)
REPRESENTATION_RELATIONSHIP_WITH_TRANSFORMATION(#83)
SHAPE_REPRESENTATION_RELATIONSHIP()
);
#223=(
REPRESENTATION_RELATIONSHIP($,$,#22687,#22639)
REPRESENTATION_RELATIONSHIP_WITH_TRANSFORMATION(#84)
SHAPE_REPRESENTATION_RELATIONSHIP()
);
#224=(
REPRESENTATION_RELATIONSHIP($,$,#22676,#22639)
REPRESENTATION_RELATIONSHIP_WITH_TRANSFORMATION(#85)
SHAPE_REPRESENTATION_RELATIONSHIP()
);
#225=(
REPRESENTATION_RELATIONSHIP($,$,#22676,#22639)
REPRESENTATION_RELATIONSHIP_WITH_TRANSFORMATION(#86)
SHAPE_REPRESENTATION_RELATIONSHIP()
);
#226=(
REPRESENTATION_RELATIONSHIP($,$,#22674,#22639)
REPRESENTATION_RELATIONSHIP_WITH_TRANSFORMATION(#87)
SHAPE_REPRESENTATION_RELATIONSHIP()
);
#227=(
REPRESENTATION_RELATIONSHIP($,$,#22675,#22639)
REPRESENTATION_RELATIONSHIP_WITH_TRANSFORMATION(#88)
SHAPE_REPRESENTATION_RELATIONSHIP()
);
#228=(
REPRESENTATION_RELATIONSHIP($,$,#22675,#22639)
REPRESENTATION_RELATIONSHIP_WITH_TRANSFORMATION(#89)
SHAPE_REPRESENTATION_RELATIONSHIP()
);
#229=(
REPRESENTATION_RELATIONSHIP($,$,#22687,#22639)
REPRESENTATION_RELATIONSHIP_WITH_TRANSFORMATION(#90)
SHAPE_REPRESENTATION_RELATIONSHIP()
);
#230=(
REPRESENTATION_RELATIONSHIP($,$,#22676,#22639)
REPRESENTATION_RELATIONSHIP_WITH_TRANSFORMATION(#91)
SHAPE_REPRESENTATION_RELATIONSHIP()
);
#231=(
REPRESENTATION_RELATIONSHIP($,$,#22676,#22639)
REPRESENTATION_RELATIONSHIP_WITH_TRANSFORMATION(#92)
SHAPE_REPRESENTATION_RELATIONSHIP()
);
#232=(
REPRESENTATION_RELATIONSHIP($,$,#22673,#22639)
REPRESENTATION_RELATIONSHIP_WITH_TRANSFORMATION(#93)
SHAPE_REPRESENTATION_RELATIONSHIP()
);
#233=(
REPRESENTATION_RELATIONSHIP($,$,#22674,#22639)
REPRESENTATION_RELATIONSHIP_WITH_TRANSFORMATION(#94)
SHAPE_REPRESENTATION_RELATIONSHIP()
);
#234=(
REPRESENTATION_RELATIONSHIP($,$,#22675,#22639)
REPRESENTATION_RELATIONSHIP_WITH_TRANSFORMATION(#95)
SHAPE_REPRESENTATION_RELATIONSHIP()
);
#235=(
REPRESENTATION_RELATIONSHIP($,$,#22675,#22639)
REPRESENTATION_RELATIONSHIP_WITH_TRANSFORMATION(#96)
SHAPE_REPRESENTATION_RELATIONSHIP()
);
#236=(
REPRESENTATION_RELATIONSHIP($,$,#22687,#22639)
REPRESENTATION_RELATIONSHIP_WITH_TRANSFORMATION(#97)
SHAPE_REPRESENTATION_RELATIONSHIP()
);
#237=(
REPRESENTATION_RELATIONSHIP($,$,#22676,#22639)
REPRESENTATION_RELATIONSHIP_WITH_TRANSFORMATION(#98)
SHAPE_REPRESENTATION_RELATIONSHIP()
);
#238=(
REPRESENTATION_RELATIONSHIP($,$,#22676,#22639)
REPRESENTATION_RELATIONSHIP_WITH_TRANSFORMATION(#99)
SHAPE_REPRESENTATION_RELATIONSHIP()
);
#239=(
REPRESENTATION_RELATIONSHIP($,$,#22674,#22639)
REPRESENTATION_RELATIONSHIP_WITH_TRANSFORMATION(#100)
SHAPE_REPRESENTATION_RELATIONSHIP()
);
#240=(
REPRESENTATION_RELATIONSHIP($,$,#22675,#22639)
REPRESENTATION_RELATIONSHIP_WITH_TRANSFORMATION(#101)
SHAPE_REPRESENTATION_RELATIONSHIP()
);
#241=(
REPRESENTATION_RELATIONSHIP($,$,#22675,#22639)
REPRESENTATION_RELATIONSHIP_WITH_TRANSFORMATION(#102)
SHAPE_REPRESENTATION_RELATIONSHIP()
);
#242=(
REPRESENTATION_RELATIONSHIP($,$,#22687,#22639)
REPRESENTATION_RELATIONSHIP_WITH_TRANSFORMATION(#103)
SHAPE_REPRESENTATION_RELATIONSHIP()
);
#243=(
REPRESENTATION_RELATIONSHIP($,$,#22676,#22639)
REPRESENTATION_RELATIONSHIP_WITH_TRANSFORMATION(#104)
SHAPE_REPRESENTATION_RELATIONSHIP()
);
#244=(
REPRESENTATION_RELATIONSHIP($,$,#22676,#22639)
REPRESENTATION_RELATIONSHIP_WITH_TRANSFORMATION(#105)
SHAPE_REPRESENTATION_RELATIONSHIP()
);
#245=(
REPRESENTATION_RELATIONSHIP($,$,#22676,#22639)
REPRESENTATION_RELATIONSHIP_WITH_TRANSFORMATION(#106)
SHAPE_REPRESENTATION_RELATIONSHIP()
);
#246=(
REPRESENTATION_RELATIONSHIP($,$,#22676,#22639)
REPRESENTATION_RELATIONSHIP_WITH_TRANSFORMATION(#107)
SHAPE_REPRESENTATION_RELATIONSHIP()
);
#247=(
REPRESENTATION_RELATIONSHIP($,$,#22676,#22639)
REPRESENTATION_RELATIONSHIP_WITH_TRANSFORMATION(#108)
SHAPE_REPRESENTATION_RELATIONSHIP()
);
#248=(
REPRESENTATION_RELATIONSHIP($,$,#22676,#22639)
REPRESENTATION_RELATIONSHIP_WITH_TRANSFORMATION(#109)
SHAPE_REPRESENTATION_RELATIONSHIP()
);
#249=(
REPRESENTATION_RELATIONSHIP($,$,#22676,#22639)
REPRESENTATION_RELATIONSHIP_WITH_TRANSFORMATION(#110)
SHAPE_REPRESENTATION_RELATIONSHIP()
);
#250=(
REPRESENTATION_RELATIONSHIP($,$,#22676,#22639)
REPRESENTATION_RELATIONSHIP_WITH_TRANSFORMATION(#111)
SHAPE_REPRESENTATION_RELATIONSHIP()
);
#251=(
REPRESENTATION_RELATIONSHIP($,$,#22676,#22639)
REPRESENTATION_RELATIONSHIP_WITH_TRANSFORMATION(#112)
SHAPE_REPRESENTATION_RELATIONSHIP()
);
#252=(
REPRESENTATION_RELATIONSHIP($,$,#22676,#22639)
REPRESENTATION_RELATIONSHIP_WITH_TRANSFORMATION(#113)
SHAPE_REPRESENTATION_RELATIONSHIP()
);
#253=(
REPRESENTATION_RELATIONSHIP($,$,#22676,#22639)
REPRESENTATION_RELATIONSHIP_WITH_TRANSFORMATION(#114)
SHAPE_REPRESENTATION_RELATIONSHIP()
);
#254=(
REPRESENTATION_RELATIONSHIP($,$,#22676,#22639)
REPRESENTATION_RELATIONSHIP_WITH_TRANSFORMATION(#115)
SHAPE_REPRESENTATION_RELATIONSHIP()
);
#255=(
REPRESENTATION_RELATIONSHIP($,$,#22676,#22639)
REPRESENTATION_RELATIONSHIP_WITH_TRANSFORMATION(#116)
SHAPE_REPRESENTATION_RELATIONSHIP()
);
#256=(
REPRESENTATION_RELATIONSHIP($,$,#22676,#22639)
REPRESENTATION_RELATIONSHIP_WITH_TRANSFORMATION(#117)
SHAPE_REPRESENTATION_RELATIONSHIP()
);
#257=(
REPRESENTATION_RELATIONSHIP($,$,#22678,#22677)
REPRESENTATION_RELATIONSHIP_WITH_TRANSFORMATION(#118)
SHAPE_REPRESENTATION_RELATIONSHIP()
);
#258=(
REPRESENTATION_RELATIONSHIP($,$,#22679,#22677)
REPRESENTATION_RELATIONSHIP_WITH_TRANSFORMATION(#119)
SHAPE_REPRESENTATION_RELATIONSHIP()
);
#259=(
REPRESENTATION_RELATIONSHIP($,$,#22680,#22677)
REPRESENTATION_RELATIONSHIP_WITH_TRANSFORMATION(#120)
SHAPE_REPRESENTATION_RELATIONSHIP()
);
#260=(
REPRESENTATION_RELATIONSHIP($,$,#22681,#22677)
REPRESENTATION_RELATIONSHIP_WITH_TRANSFORMATION(#121)
SHAPE_REPRESENTATION_RELATIONSHIP()
);
#261=(
REPRESENTATION_RELATIONSHIP($,$,#22682,#22677)
REPRESENTATION_RELATIONSHIP_WITH_TRANSFORMATION(#122)
SHAPE_REPRESENTATION_RELATIONSHIP()
);
#262=(
REPRESENTATION_RELATIONSHIP($,$,#22683,#22677)
REPRESENTATION_RELATIONSHIP_WITH_TRANSFORMATION(#123)
SHAPE_REPRESENTATION_RELATIONSHIP()
);
#263=(
REPRESENTATION_RELATIONSHIP($,$,#22684,#22677)
REPRESENTATION_RELATIONSHIP_WITH_TRANSFORMATION(#124)
SHAPE_REPRESENTATION_RELATIONSHIP()
);
#264=(
REPRESENTATION_RELATIONSHIP($,$,#22687,#22677)
REPRESENTATION_RELATIONSHIP_WITH_TRANSFORMATION(#125)
SHAPE_REPRESENTATION_RELATIONSHIP()
);
#265=(
REPRESENTATION_RELATIONSHIP($,$,#22687,#22677)
REPRESENTATION_RELATIONSHIP_WITH_TRANSFORMATION(#126)
SHAPE_REPRESENTATION_RELATIONSHIP()
);
#266=(
REPRESENTATION_RELATIONSHIP($,$,#22687,#22677)
REPRESENTATION_RELATIONSHIP_WITH_TRANSFORMATION(#127)
SHAPE_REPRESENTATION_RELATIONSHIP()
);
#267=(
REPRESENTATION_RELATIONSHIP($,$,#22687,#22677)
REPRESENTATION_RELATIONSHIP_WITH_TRANSFORMATION(#128)
SHAPE_REPRESENTATION_RELATIONSHIP()
);
#268=(
REPRESENTATION_RELATIONSHIP($,$,#22684,#22677)
REPRESENTATION_RELATIONSHIP_WITH_TRANSFORMATION(#129)
SHAPE_REPRESENTATION_RELATIONSHIP()
);
#269=(
REPRESENTATION_RELATIONSHIP($,$,#22687,#22677)
REPRESENTATION_RELATIONSHIP_WITH_TRANSFORMATION(#130)
SHAPE_REPRESENTATION_RELATIONSHIP()
);
#270=(
REPRESENTATION_RELATIONSHIP($,$,#22687,#22677)
REPRESENTATION_RELATIONSHIP_WITH_TRANSFORMATION(#131)
SHAPE_REPRESENTATION_RELATIONSHIP()
);
#271=(
REPRESENTATION_RELATIONSHIP($,$,#22687,#22677)
REPRESENTATION_RELATIONSHIP_WITH_TRANSFORMATION(#132)
SHAPE_REPRESENTATION_RELATIONSHIP()
);
#272=(
REPRESENTATION_RELATIONSHIP($,$,#22687,#22677)
REPRESENTATION_RELATIONSHIP_WITH_TRANSFORMATION(#133)
SHAPE_REPRESENTATION_RELATIONSHIP()
);
#273=(
REPRESENTATION_RELATIONSHIP($,$,#22684,#22677)
REPRESENTATION_RELATIONSHIP_WITH_TRANSFORMATION(#134)
SHAPE_REPRESENTATION_RELATIONSHIP()
);
#274=(
REPRESENTATION_RELATIONSHIP($,$,#22687,#22677)
REPRESENTATION_RELATIONSHIP_WITH_TRANSFORMATION(#135)
SHAPE_REPRESENTATION_RELATIONSHIP()
);
#275=(
REPRESENTATION_RELATIONSHIP($,$,#22687,#22677)
REPRESENTATION_RELATIONSHIP_WITH_TRANSFORMATION(#136)
SHAPE_REPRESENTATION_RELATIONSHIP()
);
#276=(
REPRESENTATION_RELATIONSHIP($,$,#22687,#22677)
REPRESENTATION_RELATIONSHIP_WITH_TRANSFORMATION(#137)
SHAPE_REPRESENTATION_RELATIONSHIP()
);
#277=(
REPRESENTATION_RELATIONSHIP($,$,#22687,#22677)
REPRESENTATION_RELATIONSHIP_WITH_TRANSFORMATION(#138)
SHAPE_REPRESENTATION_RELATIONSHIP()
);
#278=(
REPRESENTATION_RELATIONSHIP($,$,#22684,#22677)
REPRESENTATION_RELATIONSHIP_WITH_TRANSFORMATION(#139)
SHAPE_REPRESENTATION_RELATIONSHIP()
);
#279=(
REPRESENTATION_RELATIONSHIP($,$,#22687,#22677)
REPRESENTATION_RELATIONSHIP_WITH_TRANSFORMATION(#140)
SHAPE_REPRESENTATION_RELATIONSHIP()
);
#280=(
REPRESENTATION_RELATIONSHIP($,$,#22687,#22677)
REPRESENTATION_RELATIONSHIP_WITH_TRANSFORMATION(#141)
SHAPE_REPRESENTATION_RELATIONSHIP()
);
#281=(
REPRESENTATION_RELATIONSHIP($,$,#22687,#22677)
REPRESENTATION_RELATIONSHIP_WITH_TRANSFORMATION(#142)
SHAPE_REPRESENTATION_RELATIONSHIP()
);
#282=(
REPRESENTATION_RELATIONSHIP($,$,#22687,#22677)
REPRESENTATION_RELATIONSHIP_WITH_TRANSFORMATION(#143)
SHAPE_REPRESENTATION_RELATIONSHIP()
);
#283=(
REPRESENTATION_RELATIONSHIP($,$,#22687,#22677)
REPRESENTATION_RELATIONSHIP_WITH_TRANSFORMATION(#144)
SHAPE_REPRESENTATION_RELATIONSHIP()
);
#284=(
REPRESENTATION_RELATIONSHIP($,$,#22687,#22677)
REPRESENTATION_RELATIONSHIP_WITH_TRANSFORMATION(#145)
SHAPE_REPRESENTATION_RELATIONSHIP()
);
#285=(
REPRESENTATION_RELATIONSHIP($,$,#22687,#22677)
REPRESENTATION_RELATIONSHIP_WITH_TRANSFORMATION(#146)
SHAPE_REPRESENTATION_RELATIONSHIP()
);
#286=(
REPRESENTATION_RELATIONSHIP($,$,#22687,#22677)
REPRESENTATION_RELATIONSHIP_WITH_TRANSFORMATION(#147)
SHAPE_REPRESENTATION_RELATIONSHIP()
);
#287=(
REPRESENTATION_RELATIONSHIP($,$,#22639,#22638)
REPRESENTATION_RELATIONSHIP_WITH_TRANSFORMATION(#148)
SHAPE_REPRESENTATION_RELATIONSHIP()
);
#288=(
REPRESENTATION_RELATIONSHIP($,$,#22677,#22638)
REPRESENTATION_RELATIONSHIP_WITH_TRANSFORMATION(#149)
SHAPE_REPRESENTATION_RELATIONSHIP()
);
#289=CONTEXT_DEPENDENT_SHAPE_REPRESENTATION(#150,#22498);
#290=CONTEXT_DEPENDENT_SHAPE_REPRESENTATION(#151,#22499);
#291=CONTEXT_DEPENDENT_SHAPE_REPRESENTATION(#152,#22501);
#292=CONTEXT_DEPENDENT_SHAPE_REPRESENTATION(#153,#22502);
#293=CONTEXT_DEPENDENT_SHAPE_REPRESENTATION(#154,#22503);
#294=CONTEXT_DEPENDENT_SHAPE_REPRESENTATION(#155,#22504);
#295=CONTEXT_DEPENDENT_SHAPE_REPRESENTATION(#156,#22505);
#296=CONTEXT_DEPENDENT_SHAPE_REPRESENTATION(#157,#22506);
#297=CONTEXT_DEPENDENT_SHAPE_REPRESENTATION(#158,#22507);
#298=CONTEXT_DEPENDENT_SHAPE_REPRESENTATION(#159,#22508);
#299=CONTEXT_DEPENDENT_SHAPE_REPRESENTATION(#160,#22509);
#300=CONTEXT_DEPENDENT_SHAPE_REPRESENTATION(#161,#22510);
#301=CONTEXT_DEPENDENT_SHAPE_REPRESENTATION(#162,#22511);
#302=CONTEXT_DEPENDENT_SHAPE_REPRESENTATION(#163,#22512);
#303=CONTEXT_DEPENDENT_SHAPE_REPRESENTATION(#164,#22513);
#304=CONTEXT_DEPENDENT_SHAPE_REPRESENTATION(#165,#22514);
#305=CONTEXT_DEPENDENT_SHAPE_REPRESENTATION(#166,#22515);
#306=CONTEXT_DEPENDENT_SHAPE_REPRESENTATION(#167,#22516);
#307=CONTEXT_DEPENDENT_SHAPE_REPRESENTATION(#168,#22517);
#308=CONTEXT_DEPENDENT_SHAPE_REPRESENTATION(#169,#22518);
#309=CONTEXT_DEPENDENT_SHAPE_REPRESENTATION(#170,#22519);
#310=CONTEXT_DEPENDENT_SHAPE_REPRESENTATION(#171,#22520);
#311=CONTEXT_DEPENDENT_SHAPE_REPRESENTATION(#172,#22521);
#312=CONTEXT_DEPENDENT_SHAPE_REPRESENTATION(#173,#22522);
#313=CONTEXT_DEPENDENT_SHAPE_REPRESENTATION(#174,#22523);
#314=CONTEXT_DEPENDENT_SHAPE_REPRESENTATION(#175,#22524);
#315=CONTEXT_DEPENDENT_SHAPE_REPRESENTATION(#176,#22525);
#316=CONTEXT_DEPENDENT_SHAPE_REPRESENTATION(#177,#22526);
#317=CONTEXT_DEPENDENT_SHAPE_REPRESENTATION(#178,#22527);
#318=CONTEXT_DEPENDENT_SHAPE_REPRESENTATION(#179,#22528);
#319=CONTEXT_DEPENDENT_SHAPE_REPRESENTATION(#180,#22529);
#320=CONTEXT_DEPENDENT_SHAPE_REPRESENTATION(#181,#22530);
#321=CONTEXT_DEPENDENT_SHAPE_REPRESENTATION(#182,#22531);
#322=CONTEXT_DEPENDENT_SHAPE_REPRESENTATION(#183,#22532);
#323=CONTEXT_DEPENDENT_SHAPE_REPRESENTATION(#184,#22533);
#324=CONTEXT_DEPENDENT_SHAPE_REPRESENTATION(#185,#22534);
#325=CONTEXT_DEPENDENT_SHAPE_REPRESENTATION(#186,#22535);
#326=CONTEXT_DEPENDENT_SHAPE_REPRESENTATION(#187,#22536);
#327=CONTEXT_DEPENDENT_SHAPE_REPRESENTATION(#188,#22537);
#328=CONTEXT_DEPENDENT_SHAPE_REPRESENTATION(#189,#22538);
#329=CONTEXT_DEPENDENT_SHAPE_REPRESENTATION(#190,#22539);
#330=CONTEXT_DEPENDENT_SHAPE_REPRESENTATION(#191,#22540);
#331=CONTEXT_DEPENDENT_SHAPE_REPRESENTATION(#192,#22541);
#332=CONTEXT_DEPENDENT_SHAPE_REPRESENTATION(#193,#22542);
#333=CONTEXT_DEPENDENT_SHAPE_REPRESENTATION(#194,#22543);
#334=CONTEXT_DEPENDENT_SHAPE_REPRESENTATION(#195,#22544);
#335=CONTEXT_DEPENDENT_SHAPE_REPRESENTATION(#196,#22545);
#336=CONTEXT_DEPENDENT_SHAPE_REPRESENTATION(#197,#22546);
#337=CONTEXT_DEPENDENT_SHAPE_REPRESENTATION(#198,#22547);
#338=CONTEXT_DEPENDENT_SHAPE_REPRESENTATION(#199,#22548);
#339=CONTEXT_DEPENDENT_SHAPE_REPRESENTATION(#200,#22549);
#340=CONTEXT_DEPENDENT_SHAPE_REPRESENTATION(#201,#22550);
#341=CONTEXT_DEPENDENT_SHAPE_REPRESENTATION(#202,#22551);
#342=CONTEXT_DEPENDENT_SHAPE_REPRESENTATION(#203,#22552);
#343=CONTEXT_DEPENDENT_SHAPE_REPRESENTATION(#204,#22553);
#344=CONTEXT_DEPENDENT_SHAPE_REPRESENTATION(#205,#22554);
#345=CONTEXT_DEPENDENT_SHAPE_REPRESENTATION(#206,#22555);
#346=CONTEXT_DEPENDENT_SHAPE_REPRESENTATION(#207,#22556);
#347=CONTEXT_DEPENDENT_SHAPE_REPRESENTATION(#208,#22557);
#348=CONTEXT_DEPENDENT_SHAPE_REPRESENTATION(#209,#22558);
#349=CONTEXT_DEPENDENT_SHAPE_REPRESENTATION(#210,#22559);
#350=CONTEXT_DEPENDENT_SHAPE_REPRESENTATION(#211,#22560);
#351=CONTEXT_DEPENDENT_SHAPE_REPRESENTATION(#212,#22561);
#352=CONTEXT_DEPENDENT_SHAPE_REPRESENTATION(#213,#22562);
#353=CONTEXT_DEPENDENT_SHAPE_REPRESENTATION(#214,#22563);
#354=CONTEXT_DEPENDENT_SHAPE_REPRESENTATION(#215,#22564);
#355=CONTEXT_DEPENDENT_SHAPE_REPRESENTATION(#216,#22565);
#356=CONTEXT_DEPENDENT_SHAPE_REPRESENTATION(#217,#22566);
#357=CONTEXT_DEPENDENT_SHAPE_REPRESENTATION(#218,#22567);
#358=CONTEXT_DEPENDENT_SHAPE_REPRESENTATION(#219,#22568);
#359=CONTEXT_DEPENDENT_SHAPE_REPRESENTATION(#220,#22569);
#360=CONTEXT_DEPENDENT_SHAPE_REPRESENTATION(#221,#22570);
#361=CONTEXT_DEPENDENT_SHAPE_REPRESENTATION(#222,#22571);
#362=CONTEXT_DEPENDENT_SHAPE_REPRESENTATION(#223,#22572);
#363=CONTEXT_DEPENDENT_SHAPE_REPRESENTATION(#224,#22573);
#364=CONTEXT_DEPENDENT_SHAPE_REPRESENTATION(#225,#22574);
#365=CONTEXT_DEPENDENT_SHAPE_REPRESENTATION(#226,#22575);
#366=CONTEXT_DEPENDENT_SHAPE_REPRESENTATION(#227,#22576);
#367=CONTEXT_DEPENDENT_SHAPE_REPRESENTATION(#228,#22577);
#368=CONTEXT_DEPENDENT_SHAPE_REPRESENTATION(#229,#22578);
#369=CONTEXT_DEPENDENT_SHAPE_REPRESENTATION(#230,#22579);
#370=CONTEXT_DEPENDENT_SHAPE_REPRESENTATION(#231,#22580);
#371=CONTEXT_DEPENDENT_SHAPE_REPRESENTATION(#232,#22581);
#372=CONTEXT_DEPENDENT_SHAPE_REPRESENTATION(#233,#22582);
#373=CONTEXT_DEPENDENT_SHAPE_REPRESENTATION(#234,#22583);
#374=CONTEXT_DEPENDENT_SHAPE_REPRESENTATION(#235,#22584);
#375=CONTEXT_DEPENDENT_SHAPE_REPRESENTATION(#236,#22585);
#376=CONTEXT_DEPENDENT_SHAPE_REPRESENTATION(#237,#22586);
#377=CONTEXT_DEPENDENT_SHAPE_REPRESENTATION(#238,#22587);
#378=CONTEXT_DEPENDENT_SHAPE_REPRESENTATION(#239,#22588);
#379=CONTEXT_DEPENDENT_SHAPE_REPRESENTATION(#240,#22589);
#380=CONTEXT_DEPENDENT_SHAPE_REPRESENTATION(#241,#22590);
#381=CONTEXT_DEPENDENT_SHAPE_REPRESENTATION(#242,#22591);
#382=CONTEXT_DEPENDENT_SHAPE_REPRESENTATION(#243,#22592);
#383=CONTEXT_DEPENDENT_SHAPE_REPRESENTATION(#244,#22593);
#384=CONTEXT_DEPENDENT_SHAPE_REPRESENTATION(#245,#22594);
#385=CONTEXT_DEPENDENT_SHAPE_REPRESENTATION(#246,#22595);
#386=CONTEXT_DEPENDENT_SHAPE_REPRESENTATION(#247,#22596);
#387=CONTEXT_DEPENDENT_SHAPE_REPRESENTATION(#248,#22597);
#388=CONTEXT_DEPENDENT_SHAPE_REPRESENTATION(#249,#22598);
#389=CONTEXT_DEPENDENT_SHAPE_REPRESENTATION(#250,#22599);
#390=CONTEXT_DEPENDENT_SHAPE_REPRESENTATION(#251,#22600);
#391=CONTEXT_DEPENDENT_SHAPE_REPRESENTATION(#252,#22601);
#392=CONTEXT_DEPENDENT_SHAPE_REPRESENTATION(#253,#22602);
#393=CONTEXT_DEPENDENT_SHAPE_REPRESENTATION(#254,#22603);
#394=CONTEXT_DEPENDENT_SHAPE_REPRESENTATION(#255,#22604);
#395=CONTEXT_DEPENDENT_SHAPE_REPRESENTATION(#256,#22605);
#396=CONTEXT_DEPENDENT_SHAPE_REPRESENTATION(#257,#22606);
#397=CONTEXT_DEPENDENT_SHAPE_REPRESENTATION(#258,#22607);
#398=CONTEXT_DEPENDENT_SHAPE_REPRESENTATION(#259,#22608);
#399=CONTEXT_DEPENDENT_SHAPE_REPRESENTATION(#260,#22609);
#400=CONTEXT_DEPENDENT_SHAPE_REPRESENTATION(#261,#22610);
#401=CONTEXT_DEPENDENT_SHAPE_REPRESENTATION(#262,#22611);
#402=CONTEXT_DEPENDENT_SHAPE_REPRESENTATION(#263,#22612);
#403=CONTEXT_DEPENDENT_SHAPE_REPRESENTATION(#264,#22613);
#404=CONTEXT_DEPENDENT_SHAPE_REPRESENTATION(#265,#22614);
#405=CONTEXT_DEPENDENT_SHAPE_REPRESENTATION(#266,#22615);
#406=CONTEXT_DEPENDENT_SHAPE_REPRESENTATION(#267,#22616);
#407=CONTEXT_DEPENDENT_SHAPE_REPRESENTATION(#268,#22617);
#408=CONTEXT_DEPENDENT_SHAPE_REPRESENTATION(#269,#22618);
#409=CONTEXT_DEPENDENT_SHAPE_REPRESENTATION(#270,#22619);
#410=CONTEXT_DEPENDENT_SHAPE_REPRESENTATION(#271,#22620);
#411=CONTEXT_DEPENDENT_SHAPE_REPRESENTATION(#272,#22621);
#412=CONTEXT_DEPENDENT_SHAPE_REPRESENTATION(#273,#22622);
#413=CONTEXT_DEPENDENT_SHAPE_REPRESENTATION(#274,#22623);
#414=CONTEXT_DEPENDENT_SHAPE_REPRESENTATION(#275,#22624);
#415=CONTEXT_DEPENDENT_SHAPE_REPRESENTATION(#276,#22625);
#416=CONTEXT_DEPENDENT_SHAPE_REPRESENTATION(#277,#22626);
#417=CONTEXT_DEPENDENT_SHAPE_REPRESENTATION(#278,#22627);
#418=CONTEXT_DEPENDENT_SHAPE_REPRESENTATION(#279,#22628);
#419=CONTEXT_DEPENDENT_SHAPE_REPRESENTATION(#280,#22629);
#420=CONTEXT_DEPENDENT_SHAPE_REPRESENTATION(#281,#22630);
#421=CONTEXT_DEPENDENT_SHAPE_REPRESENTATION(#282,#22631);
#422=CONTEXT_DEPENDENT_SHAPE_REPRESENTATION(#283,#22632);
#423=CONTEXT_DEPENDENT_SHAPE_REPRESENTATION(#284,#22633);
#424=CONTEXT_DEPENDENT_SHAPE_REPRESENTATION(#285,#22634);
#425=CONTEXT_DEPENDENT_SHAPE_REPRESENTATION(#286,#22635);
#426=CONTEXT_DEPENDENT_SHAPE_REPRESENTATION(#287,#22636);
#427=CONTEXT_DEPENDENT_SHAPE_REPRESENTATION(#288,#22637);
#428=NEXT_ASSEMBLY_USAGE_OCCURRENCE('Steel sleeve:1','Steel sleeve:1',
'Steel sleeve:1',#22735,#22736,'Steel sleeve:1');
#429=NEXT_ASSEMBLY_USAGE_OCCURRENCE('Ball retainer (plastic):1',
'Ball retainer (plastic):1','Ball retainer (plastic):1',#22735,#22737,
'Ball retainer (plastic):1');
#430=NEXT_ASSEMBLY_USAGE_OCCURRENCE('Base:1','Base:1','Base:1',#22690,#22691,
'Base:1');
#431=NEXT_ASSEMBLY_USAGE_OCCURRENCE('Foot strip:1','Foot strip:1',
'Foot strip:1',#22690,#22692,'Foot strip:1');
#432=NEXT_ASSEMBLY_USAGE_OCCURRENCE('Foot strip (1):1',
'Foot strip (1):1','Foot strip (1):1',#22690,#22693,'Foot strip (1):1');
#433=NEXT_ASSEMBLY_USAGE_OCCURRENCE('Guide header:1','Guide header:1',
'Guide header:1',#22690,#22694,'Guide header:1');
#434=NEXT_ASSEMBLY_USAGE_OCCURRENCE('Frame upright:1','Frame upright:1',
'Frame upright:1',#22690,#22695,'Frame upright:1');
#435=NEXT_ASSEMBLY_USAGE_OCCURRENCE('Frame upright (1):1',
'Frame upright (1):1','Frame upright (1):1',#22690,#22696,
'Frame upright (1):1');
#436=NEXT_ASSEMBLY_USAGE_OCCURRENCE('Lower guide bracket:1',
'Lower guide bracket:1','Lower guide bracket:1',#22690,#22697,
'Lower guide bracket:1');
#437=NEXT_ASSEMBLY_USAGE_OCCURRENCE('Upper guide bracket:1',
'Upper guide bracket:1','Upper guide bracket:1',#22690,#22698,
'Upper guide bracket:1');
#438=NEXT_ASSEMBLY_USAGE_OCCURRENCE('Lower spring seat:1',
'Lower spring seat:1','Lower spring seat:1',#22690,#22699,
'Lower spring seat:1');
#439=NEXT_ASSEMBLY_USAGE_OCCURRENCE('Installed compression spring:1',
'Installed compression spring:1','Installed compression spring:1',#22690,
#22700,'Installed compression spring:1');
#440=NEXT_ASSEMBLY_USAGE_OCCURRENCE('Lower guide bracket (1):1',
'Lower guide bracket (1):1','Lower guide bracket (1):1',#22690,#22701,
'Lower guide bracket (1):1');
#441=NEXT_ASSEMBLY_USAGE_OCCURRENCE('Upper guide bracket (1):1',
'Upper guide bracket (1):1','Upper guide bracket (1):1',#22690,#22702,
'Upper guide bracket (1):1');
#442=NEXT_ASSEMBLY_USAGE_OCCURRENCE('Lower spring seat (1):1',
'Lower spring seat (1):1','Lower spring seat (1):1',#22690,#22703,
'Lower spring seat (1):1');
#443=NEXT_ASSEMBLY_USAGE_OCCURRENCE(
'Installed compression spring (1):1',
'Installed compression spring (1):1',
'Installed compression spring (1):1',#22690,#22704,
'Installed compression spring (1):1');
#444=NEXT_ASSEMBLY_USAGE_OCCURRENCE('Lower guide bracket (2):1',
'Lower guide bracket (2):1','Lower guide bracket (2):1',#22690,#22705,
'Lower guide bracket (2):1');
#445=NEXT_ASSEMBLY_USAGE_OCCURRENCE('Upper guide bracket (2):1',
'Upper guide bracket (2):1','Upper guide bracket (2):1',#22690,#22706,
'Upper guide bracket (2):1');
#446=NEXT_ASSEMBLY_USAGE_OCCURRENCE('Lower spring seat (2):1',
'Lower spring seat (2):1','Lower spring seat (2):1',#22690,#22707,
'Lower spring seat (2):1');
#447=NEXT_ASSEMBLY_USAGE_OCCURRENCE(
'Installed compression spring (2):1',
'Installed compression spring (2):1',
'Installed compression spring (2):1',#22690,#22708,
'Installed compression spring (2):1');
#448=NEXT_ASSEMBLY_USAGE_OCCURRENCE('Lower guide bracket (3):1',
'Lower guide bracket (3):1','Lower guide bracket (3):1',#22690,#22709,
'Lower guide bracket (3):1');
#449=NEXT_ASSEMBLY_USAGE_OCCURRENCE('Upper guide bracket (3):1',
'Upper guide bracket (3):1','Upper guide bracket (3):1',#22690,#22710,
'Upper guide bracket (3):1');
#450=NEXT_ASSEMBLY_USAGE_OCCURRENCE('Lower spring seat (3):1',
'Lower spring seat (3):1','Lower spring seat (3):1',#22690,#22711,
'Lower spring seat (3):1');
#451=NEXT_ASSEMBLY_USAGE_OCCURRENCE(
'Installed compression spring (3):1',
'Installed compression spring (3):1',
'Installed compression spring (3):1',#22690,#22712,
'Installed compression spring (3):1');
#452=NEXT_ASSEMBLY_USAGE_OCCURRENCE('Exciter envelope:1',
'Exciter envelope:1','Exciter envelope:1',#22690,#22713,
'Exciter envelope:1');
#453=NEXT_ASSEMBLY_USAGE_OCCURRENCE('Exciter base flange:1',
'Exciter base flange:1','Exciter base flange:1',#22690,#22714,
'Exciter base flange:1');
#454=NEXT_ASSEMBLY_USAGE_OCCURRENCE('Armature guide bush:1',
'Armature guide bush:1','Armature guide bush:1',#22690,#22715,
'Armature guide bush:1');
#455=NEXT_ASSEMBLY_USAGE_OCCURRENCE('Lower stop post:1',
'Lower stop post:1','Lower stop post:1',#22690,#22716,
'Lower stop post:1');
#456=NEXT_ASSEMBLY_USAGE_OCCURRENCE('Stop bumper:1','Stop bumper:1',
'Stop bumper:1',#22690,#22717,'Stop bumper:1');
#457=NEXT_ASSEMBLY_USAGE_OCCURRENCE('Upper stop post:1',
'Upper stop post:1','Upper stop post:1',#22690,#22718,
'Upper stop post:1');
#458=NEXT_ASSEMBLY_USAGE_OCCURRENCE('Stop bumper (1):1',
'Stop bumper (1):1','Stop bumper (1):1',#22690,#22719,
'Stop bumper (1):1');
#459=NEXT_ASSEMBLY_USAGE_OCCURRENCE('Lower stop post (1):1',
'Lower stop post (1):1','Lower stop post (1):1',#22690,#22720,
'Lower stop post (1):1');
#460=NEXT_ASSEMBLY_USAGE_OCCURRENCE('Stop bumper (2):1',
'Stop bumper (2):1','Stop bumper (2):1',#22690,#22721,
'Stop bumper (2):1');
#461=NEXT_ASSEMBLY_USAGE_OCCURRENCE('Upper stop post (1):1',
'Upper stop post (1):1','Upper stop post (1):1',#22690,#22722,
'Upper stop post (1):1');
#462=NEXT_ASSEMBLY_USAGE_OCCURRENCE('Stop bumper (3):1',
'Stop bumper (3):1','Stop bumper (3):1',#22690,#22723,
'Stop bumper (3):1');
#463=NEXT_ASSEMBLY_USAGE_OCCURRENCE('Cap Screw - M5x20:2',
'Cap Screw - M5x20:2','Cap Screw - M5x20:2',#22690,#22727,
'Cap Screw - M5x20:2');
#464=NEXT_ASSEMBLY_USAGE_OCCURRENCE('Cap Screw - M5x20:3',
'Cap Screw - M5x20:3','Cap Screw - M5x20:3',#22690,#22727,
'Cap Screw - M5x20:3');
#465=NEXT_ASSEMBLY_USAGE_OCCURRENCE('Cap Screw - M5x20:4',
'Cap Screw - M5x20:4','Cap Screw - M5x20:4',#22690,#22727,
'Cap Screw - M5x20:4');
#466=NEXT_ASSEMBLY_USAGE_OCCURRENCE('Cap Screw - M5x20:5',
'Cap Screw - M5x20:5','Cap Screw - M5x20:5',#22690,#22727,
'Cap Screw - M5x20:5');
#467=NEXT_ASSEMBLY_USAGE_OCCURRENCE('Cap Screw - M5x20:6',
'Cap Screw - M5x20:6','Cap Screw - M5x20:6',#22690,#22727,
'Cap Screw - M5x20:6');
#468=NEXT_ASSEMBLY_USAGE_OCCURRENCE('Cap Screw - M5x20:7',
'Cap Screw - M5x20:7','Cap Screw - M5x20:7',#22690,#22727,
'Cap Screw - M5x20:7');
#469=NEXT_ASSEMBLY_USAGE_OCCURRENCE('Cap Screw - M5x20:8',
'Cap Screw - M5x20:8','Cap Screw - M5x20:8',#22690,#22727,
'Cap Screw - M5x20:8');
#470=NEXT_ASSEMBLY_USAGE_OCCURRENCE('Cap Screw - M5x20:9',
'Cap Screw - M5x20:9','Cap Screw - M5x20:9',#22690,#22727,
'Cap Screw - M5x20:9');
#471=NEXT_ASSEMBLY_USAGE_OCCURRENCE(
'Precision Shaft - 12 mm Diameter, 300 mm Long:2',
'Precision Shaft - 12 mm Diameter, 300 mm Long:2',
'Precision Shaft - 12 mm Diameter, 300 mm Long:2',#22690,#22724,
'Precision Shaft - 12 mm Diameter, 300 mm Long:2');
#472=NEXT_ASSEMBLY_USAGE_OCCURRENCE('Shaft Support - 12 mm Bore:2',
'Shaft Support - 12 mm Bore:2','Shaft Support - 12 mm Bore:2',#22690,#22725,
'Shaft Support - 12 mm Bore:2');
#473=NEXT_ASSEMBLY_USAGE_OCCURRENCE('M5x14 Cap Screw:2',
'M5x14 Cap Screw:2','M5x14 Cap Screw:2',#22690,#22726,
'M5x14 Cap Screw:2');
#474=NEXT_ASSEMBLY_USAGE_OCCURRENCE('M5x14 Cap Screw:3',
'M5x14 Cap Screw:3','M5x14 Cap Screw:3',#22690,#22726,
'M5x14 Cap Screw:3');
#475=NEXT_ASSEMBLY_USAGE_OCCURRENCE('Cap Screw - M4x16:2',
'Cap Screw - M4x16:2','Cap Screw - M4x16:2',#22690,#22738,
'Cap Screw - M4x16:2');
#476=NEXT_ASSEMBLY_USAGE_OCCURRENCE('Cap Screw - M5x20:10',
'Cap Screw - M5x20:10','Cap Screw - M5x20:10',#22690,#22727,
'Cap Screw - M5x20:10');
#477=NEXT_ASSEMBLY_USAGE_OCCURRENCE('Cap Screw - M5x20:11',
'Cap Screw - M5x20:11','Cap Screw - M5x20:11',#22690,#22727,
'Cap Screw - M5x20:11');
#478=NEXT_ASSEMBLY_USAGE_OCCURRENCE('Shaft Support - 12 mm Bore:3',
'Shaft Support - 12 mm Bore:3','Shaft Support - 12 mm Bore:3',#22690,#22725,
'Shaft Support - 12 mm Bore:3');
#479=NEXT_ASSEMBLY_USAGE_OCCURRENCE('M5x14 Cap Screw:4',
'M5x14 Cap Screw:4','M5x14 Cap Screw:4',#22690,#22726,
'M5x14 Cap Screw:4');
#480=NEXT_ASSEMBLY_USAGE_OCCURRENCE('M5x14 Cap Screw:5',
'M5x14 Cap Screw:5','M5x14 Cap Screw:5',#22690,#22726,
'M5x14 Cap Screw:5');
#481=NEXT_ASSEMBLY_USAGE_OCCURRENCE('Cap Screw - M4x16:3',
'Cap Screw - M4x16:3','Cap Screw - M4x16:3',#22690,#22738,
'Cap Screw - M4x16:3');
#482=NEXT_ASSEMBLY_USAGE_OCCURRENCE('Cap Screw - M5x20:12',
'Cap Screw - M5x20:12','Cap Screw - M5x20:12',#22690,#22727,
'Cap Screw - M5x20:12');
#483=NEXT_ASSEMBLY_USAGE_OCCURRENCE('Cap Screw - M5x20:13',
'Cap Screw - M5x20:13','Cap Screw - M5x20:13',#22690,#22727,
'Cap Screw - M5x20:13');
#484=NEXT_ASSEMBLY_USAGE_OCCURRENCE(
'Precision Shaft - 12 mm Diameter, 300 mm Long:3',
'Precision Shaft - 12 mm Diameter, 300 mm Long:3',
'Precision Shaft - 12 mm Diameter, 300 mm Long:3',#22690,#22724,
'Precision Shaft - 12 mm Diameter, 300 mm Long:3');
#485=NEXT_ASSEMBLY_USAGE_OCCURRENCE('Shaft Support - 12 mm Bore:4',
'Shaft Support - 12 mm Bore:4','Shaft Support - 12 mm Bore:4',#22690,#22725,
'Shaft Support - 12 mm Bore:4');
#486=NEXT_ASSEMBLY_USAGE_OCCURRENCE('M5x14 Cap Screw:6',
'M5x14 Cap Screw:6','M5x14 Cap Screw:6',#22690,#22726,
'M5x14 Cap Screw:6');
#487=NEXT_ASSEMBLY_USAGE_OCCURRENCE('M5x14 Cap Screw:7',
'M5x14 Cap Screw:7','M5x14 Cap Screw:7',#22690,#22726,
'M5x14 Cap Screw:7');
#488=NEXT_ASSEMBLY_USAGE_OCCURRENCE('Cap Screw - M4x16:4',
'Cap Screw - M4x16:4','Cap Screw - M4x16:4',#22690,#22738,
'Cap Screw - M4x16:4');
#489=NEXT_ASSEMBLY_USAGE_OCCURRENCE('Cap Screw - M5x20:14',
'Cap Screw - M5x20:14','Cap Screw - M5x20:14',#22690,#22727,
'Cap Screw - M5x20:14');
#490=NEXT_ASSEMBLY_USAGE_OCCURRENCE('Cap Screw - M5x20:15',
'Cap Screw - M5x20:15','Cap Screw - M5x20:15',#22690,#22727,
'Cap Screw - M5x20:15');
#491=NEXT_ASSEMBLY_USAGE_OCCURRENCE('Shaft Support - 12 mm Bore:5',
'Shaft Support - 12 mm Bore:5','Shaft Support - 12 mm Bore:5',#22690,#22725,
'Shaft Support - 12 mm Bore:5');
#492=NEXT_ASSEMBLY_USAGE_OCCURRENCE('M5x14 Cap Screw:8',
'M5x14 Cap Screw:8','M5x14 Cap Screw:8',#22690,#22726,
'M5x14 Cap Screw:8');
#493=NEXT_ASSEMBLY_USAGE_OCCURRENCE('M5x14 Cap Screw:9',
'M5x14 Cap Screw:9','M5x14 Cap Screw:9',#22690,#22726,
'M5x14 Cap Screw:9');
#494=NEXT_ASSEMBLY_USAGE_OCCURRENCE('Cap Screw - M4x16:5',
'Cap Screw - M4x16:5','Cap Screw - M4x16:5',#22690,#22738,
'Cap Screw - M4x16:5');
#495=NEXT_ASSEMBLY_USAGE_OCCURRENCE('Cap Screw - M5x20:16',
'Cap Screw - M5x20:16','Cap Screw - M5x20:16',#22690,#22727,
'Cap Screw - M5x20:16');
#496=NEXT_ASSEMBLY_USAGE_OCCURRENCE('Cap Screw - M5x20:17',
'Cap Screw - M5x20:17','Cap Screw - M5x20:17',#22690,#22727,
'Cap Screw - M5x20:17');
#497=NEXT_ASSEMBLY_USAGE_OCCURRENCE(
'Precision Shaft - 12 mm Diameter, 300 mm Long:4',
'Precision Shaft - 12 mm Diameter, 300 mm Long:4',
'Precision Shaft - 12 mm Diameter, 300 mm Long:4',#22690,#22724,
'Precision Shaft - 12 mm Diameter, 300 mm Long:4');
#498=NEXT_ASSEMBLY_USAGE_OCCURRENCE('Shaft Support - 12 mm Bore:6',
'Shaft Support - 12 mm Bore:6','Shaft Support - 12 mm Bore:6',#22690,#22725,
'Shaft Support - 12 mm Bore:6');
#499=NEXT_ASSEMBLY_USAGE_OCCURRENCE('M5x14 Cap Screw:10',
'M5x14 Cap Screw:10','M5x14 Cap Screw:10',#22690,#22726,
'M5x14 Cap Screw:10');
#500=NEXT_ASSEMBLY_USAGE_OCCURRENCE('M5x14 Cap Screw:11',
'M5x14 Cap Screw:11','M5x14 Cap Screw:11',#22690,#22726,
'M5x14 Cap Screw:11');
#501=NEXT_ASSEMBLY_USAGE_OCCURRENCE('Cap Screw - M4x16:6',
'Cap Screw - M4x16:6','Cap Screw - M4x16:6',#22690,#22738,
'Cap Screw - M4x16:6');
#502=NEXT_ASSEMBLY_USAGE_OCCURRENCE('Cap Screw - M5x20:18',
'Cap Screw - M5x20:18','Cap Screw - M5x20:18',#22690,#22727,
'Cap Screw - M5x20:18');
#503=NEXT_ASSEMBLY_USAGE_OCCURRENCE('Cap Screw - M5x20:19',
'Cap Screw - M5x20:19','Cap Screw - M5x20:19',#22690,#22727,
'Cap Screw - M5x20:19');
#504=NEXT_ASSEMBLY_USAGE_OCCURRENCE('Shaft Support - 12 mm Bore:7',
'Shaft Support - 12 mm Bore:7','Shaft Support - 12 mm Bore:7',#22690,#22725,
'Shaft Support - 12 mm Bore:7');
#505=NEXT_ASSEMBLY_USAGE_OCCURRENCE('M5x14 Cap Screw:12',
'M5x14 Cap Screw:12','M5x14 Cap Screw:12',#22690,#22726,
'M5x14 Cap Screw:12');
#506=NEXT_ASSEMBLY_USAGE_OCCURRENCE('M5x14 Cap Screw:13',
'M5x14 Cap Screw:13','M5x14 Cap Screw:13',#22690,#22726,
'M5x14 Cap Screw:13');
#507=NEXT_ASSEMBLY_USAGE_OCCURRENCE('Cap Screw - M4x16:7',
'Cap Screw - M4x16:7','Cap Screw - M4x16:7',#22690,#22738,
'Cap Screw - M4x16:7');
#508=NEXT_ASSEMBLY_USAGE_OCCURRENCE('Cap Screw - M5x20:20',
'Cap Screw - M5x20:20','Cap Screw - M5x20:20',#22690,#22727,
'Cap Screw - M5x20:20');
#509=NEXT_ASSEMBLY_USAGE_OCCURRENCE('Cap Screw - M5x20:21',
'Cap Screw - M5x20:21','Cap Screw - M5x20:21',#22690,#22727,
'Cap Screw - M5x20:21');
#510=NEXT_ASSEMBLY_USAGE_OCCURRENCE(
'Precision Shaft - 12 mm Diameter, 300 mm Long:5',
'Precision Shaft - 12 mm Diameter, 300 mm Long:5',
'Precision Shaft - 12 mm Diameter, 300 mm Long:5',#22690,#22724,
'Precision Shaft - 12 mm Diameter, 300 mm Long:5');
#511=NEXT_ASSEMBLY_USAGE_OCCURRENCE('Shaft Support - 12 mm Bore:8',
'Shaft Support - 12 mm Bore:8','Shaft Support - 12 mm Bore:8',#22690,#22725,
'Shaft Support - 12 mm Bore:8');
#512=NEXT_ASSEMBLY_USAGE_OCCURRENCE('M5x14 Cap Screw:14',
'M5x14 Cap Screw:14','M5x14 Cap Screw:14',#22690,#22726,
'M5x14 Cap Screw:14');
#513=NEXT_ASSEMBLY_USAGE_OCCURRENCE('M5x14 Cap Screw:15',
'M5x14 Cap Screw:15','M5x14 Cap Screw:15',#22690,#22726,
'M5x14 Cap Screw:15');
#514=NEXT_ASSEMBLY_USAGE_OCCURRENCE('Cap Screw - M4x16:8',
'Cap Screw - M4x16:8','Cap Screw - M4x16:8',#22690,#22738,
'Cap Screw - M4x16:8');
#515=NEXT_ASSEMBLY_USAGE_OCCURRENCE('Cap Screw - M5x20:22',
'Cap Screw - M5x20:22','Cap Screw - M5x20:22',#22690,#22727,
'Cap Screw - M5x20:22');
#516=NEXT_ASSEMBLY_USAGE_OCCURRENCE('Cap Screw - M5x20:23',
'Cap Screw - M5x20:23','Cap Screw - M5x20:23',#22690,#22727,
'Cap Screw - M5x20:23');
#517=NEXT_ASSEMBLY_USAGE_OCCURRENCE('Shaft Support - 12 mm Bore:9',
'Shaft Support - 12 mm Bore:9','Shaft Support - 12 mm Bore:9',#22690,#22725,
'Shaft Support - 12 mm Bore:9');
#518=NEXT_ASSEMBLY_USAGE_OCCURRENCE('M5x14 Cap Screw:16',
'M5x14 Cap Screw:16','M5x14 Cap Screw:16',#22690,#22726,
'M5x14 Cap Screw:16');
#519=NEXT_ASSEMBLY_USAGE_OCCURRENCE('M5x14 Cap Screw:17',
'M5x14 Cap Screw:17','M5x14 Cap Screw:17',#22690,#22726,
'M5x14 Cap Screw:17');
#520=NEXT_ASSEMBLY_USAGE_OCCURRENCE('Cap Screw - M4x16:9',
'Cap Screw - M4x16:9','Cap Screw - M4x16:9',#22690,#22738,
'Cap Screw - M4x16:9');
#521=NEXT_ASSEMBLY_USAGE_OCCURRENCE('Cap Screw - M5x20:24',
'Cap Screw - M5x20:24','Cap Screw - M5x20:24',#22690,#22727,
'Cap Screw - M5x20:24');
#522=NEXT_ASSEMBLY_USAGE_OCCURRENCE('Cap Screw - M5x20:25',
'Cap Screw - M5x20:25','Cap Screw - M5x20:25',#22690,#22727,
'Cap Screw - M5x20:25');
#523=NEXT_ASSEMBLY_USAGE_OCCURRENCE('Cap Screw - M5x20:26',
'Cap Screw - M5x20:26','Cap Screw - M5x20:26',#22690,#22727,
'Cap Screw - M5x20:26');
#524=NEXT_ASSEMBLY_USAGE_OCCURRENCE('Cap Screw - M5x20:27',
'Cap Screw - M5x20:27','Cap Screw - M5x20:27',#22690,#22727,
'Cap Screw - M5x20:27');
#525=NEXT_ASSEMBLY_USAGE_OCCURRENCE('Cap Screw - M5x20:28',
'Cap Screw - M5x20:28','Cap Screw - M5x20:28',#22690,#22727,
'Cap Screw - M5x20:28');
#526=NEXT_ASSEMBLY_USAGE_OCCURRENCE('Cap Screw - M5x20:29',
'Cap Screw - M5x20:29','Cap Screw - M5x20:29',#22690,#22727,
'Cap Screw - M5x20:29');
#527=NEXT_ASSEMBLY_USAGE_OCCURRENCE('Cap Screw - M5x20:30',
'Cap Screw - M5x20:30','Cap Screw - M5x20:30',#22690,#22727,
'Cap Screw - M5x20:30');
#528=NEXT_ASSEMBLY_USAGE_OCCURRENCE('Cap Screw - M5x20:31',
'Cap Screw - M5x20:31','Cap Screw - M5x20:31',#22690,#22727,
'Cap Screw - M5x20:31');
#529=NEXT_ASSEMBLY_USAGE_OCCURRENCE('Cap Screw - M5x20:32',
'Cap Screw - M5x20:32','Cap Screw - M5x20:32',#22690,#22727,
'Cap Screw - M5x20:32');
#530=NEXT_ASSEMBLY_USAGE_OCCURRENCE('Cap Screw - M5x20:33',
'Cap Screw - M5x20:33','Cap Screw - M5x20:33',#22690,#22727,
'Cap Screw - M5x20:33');
#531=NEXT_ASSEMBLY_USAGE_OCCURRENCE('Cap Screw - M5x20:34',
'Cap Screw - M5x20:34','Cap Screw - M5x20:34',#22690,#22727,
'Cap Screw - M5x20:34');
#532=NEXT_ASSEMBLY_USAGE_OCCURRENCE('Cap Screw - M5x20:35',
'Cap Screw - M5x20:35','Cap Screw - M5x20:35',#22690,#22727,
'Cap Screw - M5x20:35');
#533=NEXT_ASSEMBLY_USAGE_OCCURRENCE('Cap Screw - M5x20:36',
'Cap Screw - M5x20:36','Cap Screw - M5x20:36',#22690,#22727,
'Cap Screw - M5x20:36');
#534=NEXT_ASSEMBLY_USAGE_OCCURRENCE('Cap Screw - M5x20:37',
'Cap Screw - M5x20:37','Cap Screw - M5x20:37',#22690,#22727,
'Cap Screw - M5x20:37');
#535=NEXT_ASSEMBLY_USAGE_OCCURRENCE('Table:1','Table:1','Table:1',#22728,
#22729,'Table:1');
#536=NEXT_ASSEMBLY_USAGE_OCCURRENCE(
'Bushing housing and upper spring seat:1',
'Bushing housing and upper spring seat:1',
'Bushing housing and upper spring seat:1',#22728,#22730,
'Bushing housing and upper spring seat:1');
#537=NEXT_ASSEMBLY_USAGE_OCCURRENCE(
'Bushing housing and upper spring seat (1):1',
'Bushing housing and upper spring seat (1):1',
'Bushing housing and upper spring seat (1):1',#22728,#22731,
'Bushing housing and upper spring seat (1):1');
#538=NEXT_ASSEMBLY_USAGE_OCCURRENCE(
'Bushing housing and upper spring seat (2):1',
'Bushing housing and upper spring seat (2):1',
'Bushing housing and upper spring seat (2):1',#22728,#22732,
'Bushing housing and upper spring seat (2):1');
#539=NEXT_ASSEMBLY_USAGE_OCCURRENCE(
'Bushing housing and upper spring seat (3):1',
'Bushing housing and upper spring seat (3):1',
'Bushing housing and upper spring seat (3):1',#22728,#22733,
'Bushing housing and upper spring seat (3):1');
#540=NEXT_ASSEMBLY_USAGE_OCCURRENCE('Armature:1','Armature:1',
'Armature:1',#22728,#22734,'Armature:1');
#541=NEXT_ASSEMBLY_USAGE_OCCURRENCE(
'Linear Ball Bushing - 12 x 21 x 30 mm:2',
'Linear Ball Bushing - 12 x 21 x 30 mm:2',
'Linear Ball Bushing - 12 x 21 x 30 mm:2',#22728,#22735,
'Linear Ball Bushing - 12 x 21 x 30 mm:2');
#542=NEXT_ASSEMBLY_USAGE_OCCURRENCE('Cap Screw - M4x16:10',
'Cap Screw - M4x16:10','Cap Screw - M4x16:10',#22728,#22738,
'Cap Screw - M4x16:10');
#543=NEXT_ASSEMBLY_USAGE_OCCURRENCE('Cap Screw - M4x16:11',
'Cap Screw - M4x16:11','Cap Screw - M4x16:11',#22728,#22738,
'Cap Screw - M4x16:11');
#544=NEXT_ASSEMBLY_USAGE_OCCURRENCE('Cap Screw - M4x16:12',
'Cap Screw - M4x16:12','Cap Screw - M4x16:12',#22728,#22738,
'Cap Screw - M4x16:12');
#545=NEXT_ASSEMBLY_USAGE_OCCURRENCE('Cap Screw - M4x16:13',
'Cap Screw - M4x16:13','Cap Screw - M4x16:13',#22728,#22738,
'Cap Screw - M4x16:13');
#546=NEXT_ASSEMBLY_USAGE_OCCURRENCE(
'Linear Ball Bushing - 12 x 21 x 30 mm:3',
'Linear Ball Bushing - 12 x 21 x 30 mm:3',
'Linear Ball Bushing - 12 x 21 x 30 mm:3',#22728,#22735,
'Linear Ball Bushing - 12 x 21 x 30 mm:3');
#547=NEXT_ASSEMBLY_USAGE_OCCURRENCE('Cap Screw - M4x16:14',
'Cap Screw - M4x16:14','Cap Screw - M4x16:14',#22728,#22738,
'Cap Screw - M4x16:14');
#548=NEXT_ASSEMBLY_USAGE_OCCURRENCE('Cap Screw - M4x16:15',
'Cap Screw - M4x16:15','Cap Screw - M4x16:15',#22728,#22738,
'Cap Screw - M4x16:15');
#549=NEXT_ASSEMBLY_USAGE_OCCURRENCE('Cap Screw - M4x16:16',
'Cap Screw - M4x16:16','Cap Screw - M4x16:16',#22728,#22738,
'Cap Screw - M4x16:16');
#550=NEXT_ASSEMBLY_USAGE_OCCURRENCE('Cap Screw - M4x16:17',
'Cap Screw - M4x16:17','Cap Screw - M4x16:17',#22728,#22738,
'Cap Screw - M4x16:17');
#551=NEXT_ASSEMBLY_USAGE_OCCURRENCE(
'Linear Ball Bushing - 12 x 21 x 30 mm:4',
'Linear Ball Bushing - 12 x 21 x 30 mm:4',
'Linear Ball Bushing - 12 x 21 x 30 mm:4',#22728,#22735,
'Linear Ball Bushing - 12 x 21 x 30 mm:4');
#552=NEXT_ASSEMBLY_USAGE_OCCURRENCE('Cap Screw - M4x16:18',
'Cap Screw - M4x16:18','Cap Screw - M4x16:18',#22728,#22738,
'Cap Screw - M4x16:18');
#553=NEXT_ASSEMBLY_USAGE_OCCURRENCE('Cap Screw - M4x16:19',
'Cap Screw - M4x16:19','Cap Screw - M4x16:19',#22728,#22738,
'Cap Screw - M4x16:19');
#554=NEXT_ASSEMBLY_USAGE_OCCURRENCE('Cap Screw - M4x16:20',
'Cap Screw - M4x16:20','Cap Screw - M4x16:20',#22728,#22738,
'Cap Screw - M4x16:20');
#555=NEXT_ASSEMBLY_USAGE_OCCURRENCE('Cap Screw - M4x16:21',
'Cap Screw - M4x16:21','Cap Screw - M4x16:21',#22728,#22738,
'Cap Screw - M4x16:21');
#556=NEXT_ASSEMBLY_USAGE_OCCURRENCE(
'Linear Ball Bushing - 12 x 21 x 30 mm:5',
'Linear Ball Bushing - 12 x 21 x 30 mm:5',
'Linear Ball Bushing - 12 x 21 x 30 mm:5',#22728,#22735,
'Linear Ball Bushing - 12 x 21 x 30 mm:5');
#557=NEXT_ASSEMBLY_USAGE_OCCURRENCE('Cap Screw - M4x16:22',
'Cap Screw - M4x16:22','Cap Screw - M4x16:22',#22728,#22738,
'Cap Screw - M4x16:22');
#558=NEXT_ASSEMBLY_USAGE_OCCURRENCE('Cap Screw - M4x16:23',
'Cap Screw - M4x16:23','Cap Screw - M4x16:23',#22728,#22738,
'Cap Screw - M4x16:23');
#559=NEXT_ASSEMBLY_USAGE_OCCURRENCE('Cap Screw - M4x16:24',
'Cap Screw - M4x16:24','Cap Screw - M4x16:24',#22728,#22738,
'Cap Screw - M4x16:24');
#560=NEXT_ASSEMBLY_USAGE_OCCURRENCE('Cap Screw - M4x16:25',
'Cap Screw - M4x16:25','Cap Screw - M4x16:25',#22728,#22738,
'Cap Screw - M4x16:25');
#561=NEXT_ASSEMBLY_USAGE_OCCURRENCE('Cap Screw - M4x16:26',
'Cap Screw - M4x16:26','Cap Screw - M4x16:26',#22728,#22738,
'Cap Screw - M4x16:26');
#562=NEXT_ASSEMBLY_USAGE_OCCURRENCE('Cap Screw - M4x16:27',
'Cap Screw - M4x16:27','Cap Screw - M4x16:27',#22728,#22738,
'Cap Screw - M4x16:27');
#563=NEXT_ASSEMBLY_USAGE_OCCURRENCE('Cap Screw - M4x16:28',
'Cap Screw - M4x16:28','Cap Screw - M4x16:28',#22728,#22738,
'Cap Screw - M4x16:28');
#564=NEXT_ASSEMBLY_USAGE_OCCURRENCE('Cap Screw - M4x16:29',
'Cap Screw - M4x16:29','Cap Screw - M4x16:29',#22728,#22738,
'Cap Screw - M4x16:29');
#565=NEXT_ASSEMBLY_USAGE_OCCURRENCE(
'Frame and installed return springs:1',
'Frame and installed return springs:1',
'Frame and installed return springs:1',#22689,#22690,
'Frame and installed return springs:1');
#566=NEXT_ASSEMBLY_USAGE_OCCURRENCE('Guided table and armature:1',
'Guided table and armature:1','Guided table and armature:1',#22689,#22728,
'Guided table and armature:1');
#567=ORIENTED_CLOSED_SHELL('',*,#9239,.F.);
#568=ORIENTED_CLOSED_SHELL('',*,#9242,.F.);
#569=ORIENTED_CLOSED_SHELL('',*,#9252,.F.);
#570=BREP_WITH_VOIDS('Body1',#9240,(#567));
#571=BREP_WITH_VOIDS('Body1',#9241,(#568));
#572=BREP_WITH_VOIDS('Body1',#9251,(#569));
#573=CONICAL_SURFACE('',#10340,0.55,0.785398163397448);
#574=CONICAL_SURFACE('',#10346,0.55,0.785398163397441);
#575=CONICAL_SURFACE('',#10400,0.4,0.785398163397448);
#576=CONICAL_SURFACE('',#10404,0.41,0.785398163397448);
#577=CONICAL_SURFACE('',#10408,0.26,0.463647609000806);
#578=CONICAL_SURFACE('',#10414,0.4,0.785398163397448);
#579=CONICAL_SURFACE('',#10418,0.41,0.785398163397448);
#580=CONICAL_SURFACE('',#10422,0.26,0.463647609000806);
#581=CONICAL_SURFACE('',#10426,0.225,0.785398163397448);
#582=CONICAL_SURFACE('',#10790,0.325,0.785398163397448);
#583=CONICAL_SURFACE('',#10794,0.335,0.785398163397448);
#584=CONICAL_SURFACE('',#10798,0.21,0.463647609000806);
#585=CONICAL_SURFACE('',#10802,0.18,0.785398163397448);
#586=B_SPLINE_CURVE_WITH_KNOTS('',3,(#15906,#15907,#15908,#15909,#15910,
#15911,#15912,#15913,#15914,#15915,#15916,#15917,#15918,#15919,#15920,#15921,
#15922,#15923,#15924,#15925,#15926,#15927,#15928,#15929,#15930,#15931,#15932,
#15933,#15934,#15935,#15936,#15937,#15938,#15939,#15940,#15941,#15942,#15943,
#15944,#15945,#15946,#15947,#15948,#15949,#15950,#15951,#15952,#15953,#15954,
#15955,#15956,#15957,#15958,#15959,#15960,#15961,#15962,#15963,#15964,#15965,
#15966,#15967,#15968,#15969,#15970,#15971,#15972,#15973,#15974,#15975,#15976,
#15977,#15978,#15979,#15980,#15981,#15982,#15983,#15984,#15985,#15986,#15987,
#15988,#15989,#15990,#15991,#15992,#15993,#15994,#15995,#15996,#15997,#15998,
#15999,#16000,#16001,#16002,#16003,#16004,#16005,#16006,#16007,#16008,#16009,
#16010,#16011,#16012,#16013,#16014,#16015,#16016,#16017,#16018,#16019,#16020,
#16021,#16022,#16023,#16024,#16025,#16026,#16027,#16028,#16029,#16030,#16031,
#16032,#16033,#16034,#16035,#16036,#16037,#16038,#16039),.UNSPECIFIED.,
 .F.,.F.,(4,1,1,1,1,1,1,1,1,1,1,1,1,1,1,1,1,1,1,1,1,1,1,1,1,1,1,1,1,1,1,
1,1,1,1,1,1,1,1,1,1,1,1,1,1,1,1,1,1,1,1,1,1,1,1,1,1,1,1,1,1,1,1,1,1,1,1,
1,1,1,1,1,1,1,1,1,1,1,1,1,1,1,1,1,1,1,1,1,1,1,1,1,1,1,1,1,1,1,1,1,1,1,1,
1,1,1,1,1,1,1,1,1,1,1,1,1,1,1,1,1,1,1,1,1,1,1,1,1,1,1,1,4),(0.,0.00892857142857143,
0.0178571428571429,0.0267857142857143,0.0357142857142857,0.0446428571428571,
0.0535714285714286,0.0625,0.0714285714285714,0.0803571428571428,0.0892857142857143,
0.0982142857142857,0.107142857142857,0.116071428571429,0.125,0.133928571428571,
0.142857142857143,0.150793650793651,0.154761904761905,0.156746031746032,
0.158730158730159,0.166666666666667,0.174603174603175,0.182539682539683,
0.19047619047619,0.196428571428571,0.202380952380952,0.208333333333333,
0.214285714285714,0.222222222222222,0.23015873015873,0.238095238095238,
0.241071428571429,0.244047619047619,0.25,0.255952380952381,0.261904761904762,
0.267857142857143,0.273809523809524,0.279761904761905,0.285714285714286,
0.297619047619048,0.30952380952381,0.321428571428571,0.327380952380952,
0.333333333333333,0.341269841269841,0.349206349206349,0.357142857142857,
0.365079365079365,0.373015873015873,0.380952380952381,0.386904761904762,
0.392857142857143,0.398809523809524,0.404761904761905,0.410714285714286,
0.416666666666667,0.422619047619048,0.428571428571429,0.4375,0.446428571428571,
0.455357142857143,0.459821428571429,0.464285714285714,0.470238095238095,
0.482142857142857,0.491071428571429,0.5,0.508928571428571,0.517857142857143,
0.526785714285714,0.535714285714286,0.544642857142857,0.553571428571429,
0.5625,0.571428571428571,0.580357142857143,0.589285714285714,0.598214285714286,
0.607142857142857,0.616071428571429,0.625,0.633928571428571,0.638392857142857,
0.642857142857143,0.650793650793651,0.658730158730159,0.666666666666667,
0.672619047619048,0.678571428571428,0.684523809523809,0.69047619047619,
0.696428571428571,0.702380952380952,0.708333333333333,0.714285714285714,
0.720238095238095,0.726190476190476,0.732142857142857,0.738095238095238,
0.744047619047619,0.75,0.755952380952381,0.761904761904762,0.76984126984127,
0.777777777777778,0.785714285714286,0.794642857142857,0.803571428571428,
0.8125,0.821428571428571,0.830357142857143,0.839285714285714,0.848214285714286,
0.857142857142857,0.866071428571429,0.875,0.883928571428571,0.892857142857143,
0.901785714285714,0.910714285714286,0.919642857142857,0.928571428571429,
0.9375,0.946428571428571,0.955357142857143,0.964285714285714,0.973214285714286,
0.982142857142857,0.991071428571429,1.),.UNSPECIFIED.);
#587=B_SPLINE_CURVE_WITH_KNOTS('',3,(#17470,#17471,#17472,#17473,#17474,
#17475,#17476,#17477,#17478,#17479,#17480,#17481,#17482,#17483,#17484,#17485,
#17486,#17487,#17488,#17489,#17490,#17491,#17492,#17493,#17494,#17495,#17496,
#17497,#17498,#17499,#17500,#17501,#17502,#17503,#17504,#17505,#17506,#17507,
#17508,#17509,#17510,#17511,#17512,#17513,#17514,#17515,#17516,#17517,#17518,
#17519,#17520,#17521,#17522,#17523,#17524,#17525,#17526,#17527,#17528,#17529,
#17530,#17531,#17532,#17533,#17534,#17535,#17536,#17537,#17538,#17539,#17540,
#17541,#17542,#17543,#17544,#17545,#17546,#17547,#17548,#17549,#17550,#17551,
#17552,#17553,#17554,#17555,#17556,#17557,#17558,#17559,#17560,#17561,#17562,
#17563,#17564,#17565,#17566,#17567,#17568,#17569,#17570,#17571,#17572,#17573,
#17574,#17575,#17576,#17577,#17578,#17579,#17580,#17581,#17582,#17583,#17584,
#17585,#17586,#17587,#17588,#17589,#17590,#17591,#17592,#17593,#17594,#17595,
#17596),.UNSPECIFIED.,.F.,.F.,(4,1,1,1,1,1,1,1,1,1,1,1,1,1,1,1,1,1,1,1,
1,1,1,1,1,1,1,1,1,1,1,1,1,1,1,1,1,1,1,1,1,1,1,1,1,1,1,1,1,1,1,1,1,1,1,1,
1,1,1,1,1,1,1,1,1,1,1,1,1,1,1,1,1,1,1,1,1,1,1,1,1,1,1,1,1,1,1,1,1,1,1,1,
1,1,1,1,1,1,1,1,1,1,1,1,1,1,1,1,1,1,1,1,1,1,1,1,1,1,1,1,1,1,1,1,4),(0.,
0.00892857142857143,0.0178571428571429,0.0267857142857143,0.0357142857142857,
0.0446428571428571,0.0535714285714286,0.0625,0.0714285714285714,0.0803571428571428,
0.0892857142857143,0.0982142857142857,0.107142857142857,0.116071428571429,
0.125,0.133928571428571,0.142857142857143,0.150793650793651,0.158730158730159,
0.166666666666667,0.174603174603175,0.182539682539683,0.19047619047619,
0.196428571428571,0.202380952380952,0.208333333333333,0.214285714285714,
0.222222222222222,0.23015873015873,0.238095238095238,0.244047619047619,
0.25,0.261904761904762,0.273809523809524,0.285714285714286,0.297619047619048,
0.30952380952381,0.321428571428571,0.333333333333333,0.337301587301587,
0.341269841269841,0.349206349206349,0.357142857142857,0.365079365079365,
0.373015873015873,0.380952380952381,0.386904761904762,0.392857142857143,
0.404761904761905,0.410714285714286,0.416666666666667,0.422619047619048,
0.428571428571429,0.4375,0.446428571428571,0.455357142857143,0.459821428571429,
0.464285714285714,0.470238095238095,0.476190476190476,0.482142857142857,
0.491071428571429,0.5,0.508928571428571,0.517857142857143,0.526785714285714,
0.535714285714286,0.544642857142857,0.553571428571429,0.5625,0.571428571428571,
0.580357142857143,0.589285714285714,0.598214285714286,0.607142857142857,
0.616071428571429,0.625,0.633928571428571,0.642857142857143,0.650793650793651,
0.658730158730159,0.666666666666667,0.672619047619048,0.678571428571428,
0.684523809523809,0.69047619047619,0.696428571428571,0.702380952380952,
0.708333333333333,0.714285714285714,0.720238095238095,0.726190476190476,
0.732142857142857,0.738095238095238,0.744047619047619,0.75,0.755952380952381,
0.761904761904762,0.76984126984127,0.777777777777778,0.785714285714286,
0.794642857142857,0.803571428571428,0.8125,0.821428571428571,0.830357142857143,
0.839285714285714,0.848214285714286,0.857142857142857,0.866071428571429,
0.875,0.883928571428571,0.892857142857143,0.901785714285714,0.910714285714286,
0.919642857142857,0.928571428571429,0.9375,0.946428571428571,0.955357142857143,
0.964285714285714,0.973214285714286,0.982142857142857,0.991071428571429,
1.),.UNSPECIFIED.);
#588=B_SPLINE_CURVE_WITH_KNOTS('',3,(#19137,#19138,#19139,#19140,#19141,
#19142,#19143,#19144,#19145,#19146,#19147,#19148,#19149,#19150,#19151,#19152,
#19153,#19154,#19155,#19156,#19157,#19158,#19159,#19160,#19161,#19162,#19163,
#19164,#19165,#19166,#19167,#19168,#19169,#19170,#19171,#19172,#19173,#19174,
#19175,#19176,#19177,#19178,#19179,#19180,#19181,#19182,#19183,#19184,#19185,
#19186,#19187,#19188,#19189,#19190,#19191,#19192,#19193,#19194,#19195,#19196,
#19197,#19198,#19199,#19200,#19201,#19202,#19203,#19204,#19205,#19206,#19207,
#19208,#19209,#19210,#19211,#19212,#19213,#19214,#19215,#19216,#19217,#19218,
#19219,#19220,#19221,#19222,#19223,#19224,#19225,#19226,#19227,#19228,#19229,
#19230,#19231,#19232,#19233,#19234,#19235,#19236,#19237,#19238,#19239,#19240,
#19241,#19242,#19243,#19244,#19245,#19246,#19247,#19248,#19249,#19250,#19251,
#19252,#19253,#19254,#19255,#19256,#19257,#19258,#19259,#19260,#19261,#19262,
#19263,#19264,#19265,#19266,#19267,#19268,#19269,#19270,#19271,#19272,#19273,
#19274),.UNSPECIFIED.,.F.,.F.,(4,1,1,1,1,1,1,1,1,1,1,1,1,1,1,1,1,1,1,1,
1,1,1,1,1,1,1,1,1,1,1,1,1,1,1,1,1,1,1,1,1,1,1,1,1,1,1,1,1,1,1,1,1,1,1,1,
1,1,1,1,1,1,1,1,1,1,1,1,1,1,1,1,1,1,1,1,1,1,1,1,1,1,1,1,1,1,1,1,1,1,1,1,
1,1,1,1,1,1,1,1,1,1,1,1,1,1,1,1,1,1,1,1,1,1,1,1,1,1,1,1,1,1,1,1,1,1,1,1,
1,1,1,1,1,1,1,4),(0.,0.00892857142857143,0.0178571428571429,0.0267857142857143,
0.0357142857142857,0.0446428571428571,0.0535714285714286,0.0625,0.0714285714285714,
0.0803571428571428,0.0892857142857143,0.0982142857142857,0.107142857142857,
0.116071428571429,0.125,0.133928571428571,0.142857142857143,0.150793650793651,
0.154761904761905,0.156746031746032,0.158730158730159,0.166666666666667,
0.174603174603175,0.182539682539683,0.19047619047619,0.196428571428571,
0.202380952380952,0.208333333333333,0.214285714285714,0.222222222222222,
0.23015873015873,0.238095238095238,0.241071428571429,0.244047619047619,
0.25,0.255952380952381,0.261904761904762,0.267857142857143,0.273809523809524,
0.279761904761905,0.285714285714286,0.297619047619048,0.30952380952381,
0.321428571428571,0.327380952380952,0.333333333333333,0.341269841269841,
0.349206349206349,0.357142857142857,0.361111111111111,0.363095238095238,
0.365079365079365,0.373015873015873,0.380952380952381,0.386904761904762,
0.392857142857143,0.398809523809524,0.404761904761905,0.410714285714286,
0.416666666666667,0.422619047619048,0.428571428571429,0.4375,0.446428571428571,
0.455357142857143,0.459821428571429,0.464285714285714,0.470238095238095,
0.476190476190476,0.482142857142857,0.491071428571429,0.5,0.508928571428571,
0.517857142857143,0.526785714285714,0.535714285714286,0.544642857142857,
0.553571428571429,0.5625,0.571428571428571,0.580357142857143,0.589285714285714,
0.598214285714286,0.607142857142857,0.616071428571429,0.625,0.633928571428571,
0.642857142857143,0.650793650793651,0.658730158730159,0.666666666666667,
0.672619047619048,0.678571428571428,0.684523809523809,0.69047619047619,
0.696428571428571,0.702380952380952,0.708333333333333,0.714285714285714,
0.720238095238095,0.726190476190476,0.732142857142857,0.738095238095238,
0.744047619047619,0.75,0.755952380952381,0.761904761904762,0.76984126984127,
0.777777777777778,0.785714285714286,0.787946428571428,0.790178571428571,
0.794642857142857,0.803571428571428,0.8125,0.821428571428571,0.830357142857143,
0.839285714285714,0.848214285714286,0.857142857142857,0.866071428571429,
0.875,0.883928571428571,0.892857142857143,0.901785714285714,0.910714285714286,
0.919642857142857,0.928571428571429,0.9375,0.946428571428571,0.955357142857143,
0.964285714285714,0.973214285714286,0.982142857142857,0.991071428571429,
1.),.UNSPECIFIED.);
#589=B_SPLINE_CURVE_WITH_KNOTS('',3,(#20705,#20706,#20707,#20708,#20709,
#20710,#20711,#20712,#20713,#20714,#20715,#20716,#20717,#20718,#20719,#20720,
#20721,#20722,#20723,#20724,#20725,#20726,#20727,#20728,#20729,#20730,#20731,
#20732,#20733,#20734,#20735,#20736,#20737,#20738,#20739,#20740,#20741,#20742,
#20743,#20744,#20745,#20746,#20747,#20748,#20749,#20750,#20751,#20752,#20753,
#20754,#20755,#20756,#20757,#20758,#20759,#20760,#20761,#20762,#20763,#20764,
#20765,#20766,#20767,#20768,#20769,#20770,#20771,#20772,#20773,#20774,#20775,
#20776,#20777,#20778,#20779,#20780,#20781,#20782,#20783,#20784,#20785,#20786,
#20787,#20788,#20789,#20790,#20791,#20792,#20793,#20794,#20795,#20796,#20797,
#20798,#20799,#20800,#20801,#20802,#20803,#20804,#20805,#20806,#20807,#20808,
#20809,#20810,#20811,#20812,#20813,#20814,#20815,#20816,#20817,#20818,#20819,
#20820,#20821,#20822,#20823,#20824,#20825,#20826,#20827,#20828,#20829,#20830,
#20831),.UNSPECIFIED.,.F.,.F.,(4,1,1,1,1,1,1,1,1,1,1,1,1,1,1,1,1,1,1,1,
1,1,1,1,1,1,1,1,1,1,1,1,1,1,1,1,1,1,1,1,1,1,1,1,1,1,1,1,1,1,1,1,1,1,1,1,
1,1,1,1,1,1,1,1,1,1,1,1,1,1,1,1,1,1,1,1,1,1,1,1,1,1,1,1,1,1,1,1,1,1,1,1,
1,1,1,1,1,1,1,1,1,1,1,1,1,1,1,1,1,1,1,1,1,1,1,1,1,1,1,1,1,1,1,1,4),(0.,
0.00892857142857143,0.0178571428571429,0.0267857142857143,0.0357142857142857,
0.0446428571428571,0.0535714285714286,0.0625,0.0714285714285714,0.0803571428571428,
0.0892857142857143,0.0982142857142857,0.107142857142857,0.116071428571429,
0.125,0.133928571428571,0.142857142857143,0.150793650793651,0.158730158730159,
0.166666666666667,0.174603174603175,0.182539682539683,0.19047619047619,
0.196428571428571,0.202380952380952,0.208333333333333,0.214285714285714,
0.222222222222222,0.23015873015873,0.238095238095238,0.244047619047619,
0.25,0.261904761904762,0.273809523809524,0.285714285714286,0.297619047619048,
0.30952380952381,0.321428571428571,0.333333333333333,0.337301587301587,
0.341269841269841,0.349206349206349,0.357142857142857,0.365079365079365,
0.373015873015873,0.380952380952381,0.386904761904762,0.392857142857143,
0.404761904761905,0.410714285714286,0.416666666666667,0.422619047619048,
0.428571428571429,0.4375,0.446428571428571,0.455357142857143,0.459821428571429,
0.464285714285714,0.470238095238095,0.476190476190476,0.482142857142857,
0.491071428571429,0.5,0.508928571428571,0.517857142857143,0.526785714285714,
0.535714285714286,0.544642857142857,0.553571428571429,0.5625,0.571428571428571,
0.580357142857143,0.589285714285714,0.598214285714286,0.607142857142857,
0.616071428571429,0.625,0.633928571428571,0.642857142857143,0.650793650793651,
0.658730158730159,0.666666666666667,0.672619047619048,0.678571428571428,
0.684523809523809,0.69047619047619,0.696428571428571,0.702380952380952,
0.708333333333333,0.714285714285714,0.720238095238095,0.726190476190476,
0.732142857142857,0.738095238095238,0.744047619047619,0.75,0.755952380952381,
0.761904761904762,0.76984126984127,0.777777777777778,0.785714285714286,
0.794642857142857,0.803571428571428,0.8125,0.821428571428571,0.830357142857143,
0.839285714285714,0.848214285714286,0.857142857142857,0.866071428571429,
0.875,0.883928571428571,0.892857142857143,0.901785714285714,0.910714285714286,
0.919642857142857,0.928571428571429,0.9375,0.946428571428571,0.955357142857143,
0.964285714285714,0.973214285714286,0.982142857142857,0.991071428571429,
1.),.UNSPECIFIED.);
#590=B_SPLINE_SURFACE_WITH_KNOTS('',3,3,((#14563,#14564,#14565,#14566,#14567,
#14568,#14569,#14570,#14571,#14572,#14573,#14574,#14575,#14576,#14577,#14578,
#14579,#14580,#14581,#14582,#14583,#14584,#14585,#14586,#14587,#14588,#14589,
#14590,#14591,#14592,#14593,#14594,#14595,#14596,#14597,#14598,#14599,#14600,
#14601,#14602,#14603,#14604,#14605,#14606,#14607,#14608,#14609,#14610,#14611,
#14612,#14613,#14614,#14615,#14616,#14617,#14618,#14619,#14620,#14621,#14622,
#14623,#14624,#14625,#14626,#14627,#14628,#14629,#14630,#14631,#14632,#14633,
#14634,#14635,#14636,#14637,#14638,#14639,#14640,#14641,#14642,#14643,#14644,
#14645,#14646,#14647,#14648,#14649,#14650,#14651,#14652,#14653,#14654,#14655,
#14656,#14657,#14658,#14659,#14660,#14661,#14662,#14663,#14664,#14665,#14666,
#14667,#14668,#14669,#14670,#14671,#14672,#14673,#14674,#14675,#14676,#14677,
#14678,#14679,#14680,#14681,#14682,#14683,#14684,#14685,#14686,#14687,#14688,
#14689,#14690,#14691,#14692,#14693,#14694,#14695,#14696),(#14697,#14698,
#14699,#14700,#14701,#14702,#14703,#14704,#14705,#14706,#14707,#14708,#14709,
#14710,#14711,#14712,#14713,#14714,#14715,#14716,#14717,#14718,#14719,#14720,
#14721,#14722,#14723,#14724,#14725,#14726,#14727,#14728,#14729,#14730,#14731,
#14732,#14733,#14734,#14735,#14736,#14737,#14738,#14739,#14740,#14741,#14742,
#14743,#14744,#14745,#14746,#14747,#14748,#14749,#14750,#14751,#14752,#14753,
#14754,#14755,#14756,#14757,#14758,#14759,#14760,#14761,#14762,#14763,#14764,
#14765,#14766,#14767,#14768,#14769,#14770,#14771,#14772,#14773,#14774,#14775,
#14776,#14777,#14778,#14779,#14780,#14781,#14782,#14783,#14784,#14785,#14786,
#14787,#14788,#14789,#14790,#14791,#14792,#14793,#14794,#14795,#14796,#14797,
#14798,#14799,#14800,#14801,#14802,#14803,#14804,#14805,#14806,#14807,#14808,
#14809,#14810,#14811,#14812,#14813,#14814,#14815,#14816,#14817,#14818,#14819,
#14820,#14821,#14822,#14823,#14824,#14825,#14826,#14827,#14828,#14829,#14830),
(#14831,#14832,#14833,#14834,#14835,#14836,#14837,#14838,#14839,#14840,
#14841,#14842,#14843,#14844,#14845,#14846,#14847,#14848,#14849,#14850,#14851,
#14852,#14853,#14854,#14855,#14856,#14857,#14858,#14859,#14860,#14861,#14862,
#14863,#14864,#14865,#14866,#14867,#14868,#14869,#14870,#14871,#14872,#14873,
#14874,#14875,#14876,#14877,#14878,#14879,#14880,#14881,#14882,#14883,#14884,
#14885,#14886,#14887,#14888,#14889,#14890,#14891,#14892,#14893,#14894,#14895,
#14896,#14897,#14898,#14899,#14900,#14901,#14902,#14903,#14904,#14905,#14906,
#14907,#14908,#14909,#14910,#14911,#14912,#14913,#14914,#14915,#14916,#14917,
#14918,#14919,#14920,#14921,#14922,#14923,#14924,#14925,#14926,#14927,#14928,
#14929,#14930,#14931,#14932,#14933,#14934,#14935,#14936,#14937,#14938,#14939,
#14940,#14941,#14942,#14943,#14944,#14945,#14946,#14947,#14948,#14949,#14950,
#14951,#14952,#14953,#14954,#14955,#14956,#14957,#14958,#14959,#14960,#14961,
#14962,#14963,#14964),(#14965,#14966,#14967,#14968,#14969,#14970,#14971,
#14972,#14973,#14974,#14975,#14976,#14977,#14978,#14979,#14980,#14981,#14982,
#14983,#14984,#14985,#14986,#14987,#14988,#14989,#14990,#14991,#14992,#14993,
#14994,#14995,#14996,#14997,#14998,#14999,#15000,#15001,#15002,#15003,#15004,
#15005,#15006,#15007,#15008,#15009,#15010,#15011,#15012,#15013,#15014,#15015,
#15016,#15017,#15018,#15019,#15020,#15021,#15022,#15023,#15024,#15025,#15026,
#15027,#15028,#15029,#15030,#15031,#15032,#15033,#15034,#15035,#15036,#15037,
#15038,#15039,#15040,#15041,#15042,#15043,#15044,#15045,#15046,#15047,#15048,
#15049,#15050,#15051,#15052,#15053,#15054,#15055,#15056,#15057,#15058,#15059,
#15060,#15061,#15062,#15063,#15064,#15065,#15066,#15067,#15068,#15069,#15070,
#15071,#15072,#15073,#15074,#15075,#15076,#15077,#15078,#15079,#15080,#15081,
#15082,#15083,#15084,#15085,#15086,#15087,#15088,#15089,#15090,#15091,#15092,
#15093,#15094,#15095,#15096,#15097,#15098),(#15099,#15100,#15101,#15102,
#15103,#15104,#15105,#15106,#15107,#15108,#15109,#15110,#15111,#15112,#15113,
#15114,#15115,#15116,#15117,#15118,#15119,#15120,#15121,#15122,#15123,#15124,
#15125,#15126,#15127,#15128,#15129,#15130,#15131,#15132,#15133,#15134,#15135,
#15136,#15137,#15138,#15139,#15140,#15141,#15142,#15143,#15144,#15145,#15146,
#15147,#15148,#15149,#15150,#15151,#15152,#15153,#15154,#15155,#15156,#15157,
#15158,#15159,#15160,#15161,#15162,#15163,#15164,#15165,#15166,#15167,#15168,
#15169,#15170,#15171,#15172,#15173,#15174,#15175,#15176,#15177,#15178,#15179,
#15180,#15181,#15182,#15183,#15184,#15185,#15186,#15187,#15188,#15189,#15190,
#15191,#15192,#15193,#15194,#15195,#15196,#15197,#15198,#15199,#15200,#15201,
#15202,#15203,#15204,#15205,#15206,#15207,#15208,#15209,#15210,#15211,#15212,
#15213,#15214,#15215,#15216,#15217,#15218,#15219,#15220,#15221,#15222,#15223,
#15224,#15225,#15226,#15227,#15228,#15229,#15230,#15231,#15232),(#15233,
#15234,#15235,#15236,#15237,#15238,#15239,#15240,#15241,#15242,#15243,#15244,
#15245,#15246,#15247,#15248,#15249,#15250,#15251,#15252,#15253,#15254,#15255,
#15256,#15257,#15258,#15259,#15260,#15261,#15262,#15263,#15264,#15265,#15266,
#15267,#15268,#15269,#15270,#15271,#15272,#15273,#15274,#15275,#15276,#15277,
#15278,#15279,#15280,#15281,#15282,#15283,#15284,#15285,#15286,#15287,#15288,
#15289,#15290,#15291,#15292,#15293,#15294,#15295,#15296,#15297,#15298,#15299,
#15300,#15301,#15302,#15303,#15304,#15305,#15306,#15307,#15308,#15309,#15310,
#15311,#15312,#15313,#15314,#15315,#15316,#15317,#15318,#15319,#15320,#15321,
#15322,#15323,#15324,#15325,#15326,#15327,#15328,#15329,#15330,#15331,#15332,
#15333,#15334,#15335,#15336,#15337,#15338,#15339,#15340,#15341,#15342,#15343,
#15344,#15345,#15346,#15347,#15348,#15349,#15350,#15351,#15352,#15353,#15354,
#15355,#15356,#15357,#15358,#15359,#15360,#15361,#15362,#15363,#15364,#15365,
#15366),(#15367,#15368,#15369,#15370,#15371,#15372,#15373,#15374,#15375,
#15376,#15377,#15378,#15379,#15380,#15381,#15382,#15383,#15384,#15385,#15386,
#15387,#15388,#15389,#15390,#15391,#15392,#15393,#15394,#15395,#15396,#15397,
#15398,#15399,#15400,#15401,#15402,#15403,#15404,#15405,#15406,#15407,#15408,
#15409,#15410,#15411,#15412,#15413,#15414,#15415,#15416,#15417,#15418,#15419,
#15420,#15421,#15422,#15423,#15424,#15425,#15426,#15427,#15428,#15429,#15430,
#15431,#15432,#15433,#15434,#15435,#15436,#15437,#15438,#15439,#15440,#15441,
#15442,#15443,#15444,#15445,#15446,#15447,#15448,#15449,#15450,#15451,#15452,
#15453,#15454,#15455,#15456,#15457,#15458,#15459,#15460,#15461,#15462,#15463,
#15464,#15465,#15466,#15467,#15468,#15469,#15470,#15471,#15472,#15473,#15474,
#15475,#15476,#15477,#15478,#15479,#15480,#15481,#15482,#15483,#15484,#15485,
#15486,#15487,#15488,#15489,#15490,#15491,#15492,#15493,#15494,#15495,#15496,
#15497,#15498,#15499,#15500),(#15501,#15502,#15503,#15504,#15505,#15506,
#15507,#15508,#15509,#15510,#15511,#15512,#15513,#15514,#15515,#15516,#15517,
#15518,#15519,#15520,#15521,#15522,#15523,#15524,#15525,#15526,#15527,#15528,
#15529,#15530,#15531,#15532,#15533,#15534,#15535,#15536,#15537,#15538,#15539,
#15540,#15541,#15542,#15543,#15544,#15545,#15546,#15547,#15548,#15549,#15550,
#15551,#15552,#15553,#15554,#15555,#15556,#15557,#15558,#15559,#15560,#15561,
#15562,#15563,#15564,#15565,#15566,#15567,#15568,#15569,#15570,#15571,#15572,
#15573,#15574,#15575,#15576,#15577,#15578,#15579,#15580,#15581,#15582,#15583,
#15584,#15585,#15586,#15587,#15588,#15589,#15590,#15591,#15592,#15593,#15594,
#15595,#15596,#15597,#15598,#15599,#15600,#15601,#15602,#15603,#15604,#15605,
#15606,#15607,#15608,#15609,#15610,#15611,#15612,#15613,#15614,#15615,#15616,
#15617,#15618,#15619,#15620,#15621,#15622,#15623,#15624,#15625,#15626,#15627,
#15628,#15629,#15630,#15631,#15632,#15633,#15634),(#15635,#15636,#15637,
#15638,#15639,#15640,#15641,#15642,#15643,#15644,#15645,#15646,#15647,#15648,
#15649,#15650,#15651,#15652,#15653,#15654,#15655,#15656,#15657,#15658,#15659,
#15660,#15661,#15662,#15663,#15664,#15665,#15666,#15667,#15668,#15669,#15670,
#15671,#15672,#15673,#15674,#15675,#15676,#15677,#15678,#15679,#15680,#15681,
#15682,#15683,#15684,#15685,#15686,#15687,#15688,#15689,#15690,#15691,#15692,
#15693,#15694,#15695,#15696,#15697,#15698,#15699,#15700,#15701,#15702,#15703,
#15704,#15705,#15706,#15707,#15708,#15709,#15710,#15711,#15712,#15713,#15714,
#15715,#15716,#15717,#15718,#15719,#15720,#15721,#15722,#15723,#15724,#15725,
#15726,#15727,#15728,#15729,#15730,#15731,#15732,#15733,#15734,#15735,#15736,
#15737,#15738,#15739,#15740,#15741,#15742,#15743,#15744,#15745,#15746,#15747,
#15748,#15749,#15750,#15751,#15752,#15753,#15754,#15755,#15756,#15757,#15758,
#15759,#15760,#15761,#15762,#15763,#15764,#15765,#15766,#15767,#15768),
(#15769,#15770,#15771,#15772,#15773,#15774,#15775,#15776,#15777,#15778,
#15779,#15780,#15781,#15782,#15783,#15784,#15785,#15786,#15787,#15788,#15789,
#15790,#15791,#15792,#15793,#15794,#15795,#15796,#15797,#15798,#15799,#15800,
#15801,#15802,#15803,#15804,#15805,#15806,#15807,#15808,#15809,#15810,#15811,
#15812,#15813,#15814,#15815,#15816,#15817,#15818,#15819,#15820,#15821,#15822,
#15823,#15824,#15825,#15826,#15827,#15828,#15829,#15830,#15831,#15832,#15833,
#15834,#15835,#15836,#15837,#15838,#15839,#15840,#15841,#15842,#15843,#15844,
#15845,#15846,#15847,#15848,#15849,#15850,#15851,#15852,#15853,#15854,#15855,
#15856,#15857,#15858,#15859,#15860,#15861,#15862,#15863,#15864,#15865,#15866,
#15867,#15868,#15869,#15870,#15871,#15872,#15873,#15874,#15875,#15876,#15877,
#15878,#15879,#15880,#15881,#15882,#15883,#15884,#15885,#15886,#15887,#15888,
#15889,#15890,#15891,#15892,#15893,#15894,#15895,#15896,#15897,#15898,#15899,
#15900,#15901,#15902)),.UNSPECIFIED.,.T.,.F.,.F.,(4,1,1,1,1,1,1,4),(4,1,
1,1,1,1,1,1,1,1,1,1,1,1,1,1,1,1,1,1,1,1,1,1,1,1,1,1,1,1,1,1,1,1,1,1,1,1,
1,1,1,1,1,1,1,1,1,1,1,1,1,1,1,1,1,1,1,1,1,1,1,1,1,1,1,1,1,1,1,1,1,1,1,1,
1,1,1,1,1,1,1,1,1,1,1,1,1,1,1,1,1,1,1,1,1,1,1,1,1,1,1,1,1,1,1,1,1,1,1,1,
1,1,1,1,1,1,1,1,1,1,1,1,1,1,1,1,1,1,1,1,1,4),(-3.14159265358979,-2.24399475256414,
-1.34639685153848,-0.448798950512828,0.448798950512828,1.34639685153848,
2.24399475256414,3.14159265358979),(0.,0.00892857142857143,0.0178571428571429,
0.0267857142857143,0.0357142857142857,0.0446428571428571,0.0535714285714286,
0.0625,0.0714285714285714,0.0803571428571428,0.0892857142857143,0.0982142857142857,
0.107142857142857,0.116071428571429,0.125,0.133928571428571,0.142857142857143,
0.150793650793651,0.154761904761905,0.156746031746032,0.158730158730159,
0.166666666666667,0.174603174603175,0.182539682539683,0.19047619047619,
0.196428571428571,0.202380952380952,0.208333333333333,0.214285714285714,
0.222222222222222,0.23015873015873,0.238095238095238,0.241071428571429,
0.244047619047619,0.25,0.255952380952381,0.261904761904762,0.267857142857143,
0.273809523809524,0.279761904761905,0.285714285714286,0.297619047619048,
0.30952380952381,0.321428571428571,0.327380952380952,0.333333333333333,
0.341269841269841,0.349206349206349,0.357142857142857,0.365079365079365,
0.373015873015873,0.380952380952381,0.386904761904762,0.392857142857143,
0.398809523809524,0.404761904761905,0.410714285714286,0.416666666666667,
0.422619047619048,0.428571428571429,0.4375,0.446428571428571,0.455357142857143,
0.459821428571429,0.464285714285714,0.470238095238095,0.482142857142857,
0.491071428571429,0.5,0.508928571428571,0.517857142857143,0.526785714285714,
0.535714285714286,0.544642857142857,0.553571428571429,0.5625,0.571428571428571,
0.580357142857143,0.589285714285714,0.598214285714286,0.607142857142857,
0.616071428571429,0.625,0.633928571428571,0.638392857142857,0.642857142857143,
0.650793650793651,0.658730158730159,0.666666666666667,0.672619047619048,
0.678571428571428,0.684523809523809,0.69047619047619,0.696428571428571,
0.702380952380952,0.708333333333333,0.714285714285714,0.720238095238095,
0.726190476190476,0.732142857142857,0.738095238095238,0.744047619047619,
0.75,0.755952380952381,0.761904761904762,0.76984126984127,0.777777777777778,
0.785714285714286,0.794642857142857,0.803571428571428,0.8125,0.821428571428571,
0.830357142857143,0.839285714285714,0.848214285714286,0.857142857142857,
0.866071428571429,0.875,0.883928571428571,0.892857142857143,0.901785714285714,
0.910714285714286,0.919642857142857,0.928571428571429,0.9375,0.946428571428571,
0.955357142857143,0.964285714285714,0.973214285714286,0.982142857142857,
0.991071428571429,1.),.UNSPECIFIED.);
#591=B_SPLINE_SURFACE_WITH_KNOTS('',3,3,((#16197,#16198,#16199,#16200,#16201,
#16202,#16203,#16204,#16205,#16206,#16207,#16208,#16209,#16210,#16211,#16212,
#16213,#16214,#16215,#16216,#16217,#16218,#16219,#16220,#16221,#16222,#16223,
#16224,#16225,#16226,#16227,#16228,#16229,#16230,#16231,#16232,#16233,#16234,
#16235,#16236,#16237,#16238,#16239,#16240,#16241,#16242,#16243,#16244,#16245,
#16246,#16247,#16248,#16249,#16250,#16251,#16252,#16253,#16254,#16255,#16256,
#16257,#16258,#16259,#16260,#16261,#16262,#16263,#16264,#16265,#16266,#16267,
#16268,#16269,#16270,#16271,#16272,#16273,#16274,#16275,#16276,#16277,#16278,
#16279,#16280,#16281,#16282,#16283,#16284,#16285,#16286,#16287,#16288,#16289,
#16290,#16291,#16292,#16293,#16294,#16295,#16296,#16297,#16298,#16299,#16300,
#16301,#16302,#16303,#16304,#16305,#16306,#16307,#16308,#16309,#16310,#16311,
#16312,#16313,#16314,#16315,#16316,#16317,#16318,#16319,#16320,#16321,#16322,
#16323),(#16324,#16325,#16326,#16327,#16328,#16329,#16330,#16331,#16332,
#16333,#16334,#16335,#16336,#16337,#16338,#16339,#16340,#16341,#16342,#16343,
#16344,#16345,#16346,#16347,#16348,#16349,#16350,#16351,#16352,#16353,#16354,
#16355,#16356,#16357,#16358,#16359,#16360,#16361,#16362,#16363,#16364,#16365,
#16366,#16367,#16368,#16369,#16370,#16371,#16372,#16373,#16374,#16375,#16376,
#16377,#16378,#16379,#16380,#16381,#16382,#16383,#16384,#16385,#16386,#16387,
#16388,#16389,#16390,#16391,#16392,#16393,#16394,#16395,#16396,#16397,#16398,
#16399,#16400,#16401,#16402,#16403,#16404,#16405,#16406,#16407,#16408,#16409,
#16410,#16411,#16412,#16413,#16414,#16415,#16416,#16417,#16418,#16419,#16420,
#16421,#16422,#16423,#16424,#16425,#16426,#16427,#16428,#16429,#16430,#16431,
#16432,#16433,#16434,#16435,#16436,#16437,#16438,#16439,#16440,#16441,#16442,
#16443,#16444,#16445,#16446,#16447,#16448,#16449,#16450),(#16451,#16452,
#16453,#16454,#16455,#16456,#16457,#16458,#16459,#16460,#16461,#16462,#16463,
#16464,#16465,#16466,#16467,#16468,#16469,#16470,#16471,#16472,#16473,#16474,
#16475,#16476,#16477,#16478,#16479,#16480,#16481,#16482,#16483,#16484,#16485,
#16486,#16487,#16488,#16489,#16490,#16491,#16492,#16493,#16494,#16495,#16496,
#16497,#16498,#16499,#16500,#16501,#16502,#16503,#16504,#16505,#16506,#16507,
#16508,#16509,#16510,#16511,#16512,#16513,#16514,#16515,#16516,#16517,#16518,
#16519,#16520,#16521,#16522,#16523,#16524,#16525,#16526,#16527,#16528,#16529,
#16530,#16531,#16532,#16533,#16534,#16535,#16536,#16537,#16538,#16539,#16540,
#16541,#16542,#16543,#16544,#16545,#16546,#16547,#16548,#16549,#16550,#16551,
#16552,#16553,#16554,#16555,#16556,#16557,#16558,#16559,#16560,#16561,#16562,
#16563,#16564,#16565,#16566,#16567,#16568,#16569,#16570,#16571,#16572,#16573,
#16574,#16575,#16576,#16577),(#16578,#16579,#16580,#16581,#16582,#16583,
#16584,#16585,#16586,#16587,#16588,#16589,#16590,#16591,#16592,#16593,#16594,
#16595,#16596,#16597,#16598,#16599,#16600,#16601,#16602,#16603,#16604,#16605,
#16606,#16607,#16608,#16609,#16610,#16611,#16612,#16613,#16614,#16615,#16616,
#16617,#16618,#16619,#16620,#16621,#16622,#16623,#16624,#16625,#16626,#16627,
#16628,#16629,#16630,#16631,#16632,#16633,#16634,#16635,#16636,#16637,#16638,
#16639,#16640,#16641,#16642,#16643,#16644,#16645,#16646,#16647,#16648,#16649,
#16650,#16651,#16652,#16653,#16654,#16655,#16656,#16657,#16658,#16659,#16660,
#16661,#16662,#16663,#16664,#16665,#16666,#16667,#16668,#16669,#16670,#16671,
#16672,#16673,#16674,#16675,#16676,#16677,#16678,#16679,#16680,#16681,#16682,
#16683,#16684,#16685,#16686,#16687,#16688,#16689,#16690,#16691,#16692,#16693,
#16694,#16695,#16696,#16697,#16698,#16699,#16700,#16701,#16702,#16703,#16704),
(#16705,#16706,#16707,#16708,#16709,#16710,#16711,#16712,#16713,#16714,
#16715,#16716,#16717,#16718,#16719,#16720,#16721,#16722,#16723,#16724,#16725,
#16726,#16727,#16728,#16729,#16730,#16731,#16732,#16733,#16734,#16735,#16736,
#16737,#16738,#16739,#16740,#16741,#16742,#16743,#16744,#16745,#16746,#16747,
#16748,#16749,#16750,#16751,#16752,#16753,#16754,#16755,#16756,#16757,#16758,
#16759,#16760,#16761,#16762,#16763,#16764,#16765,#16766,#16767,#16768,#16769,
#16770,#16771,#16772,#16773,#16774,#16775,#16776,#16777,#16778,#16779,#16780,
#16781,#16782,#16783,#16784,#16785,#16786,#16787,#16788,#16789,#16790,#16791,
#16792,#16793,#16794,#16795,#16796,#16797,#16798,#16799,#16800,#16801,#16802,
#16803,#16804,#16805,#16806,#16807,#16808,#16809,#16810,#16811,#16812,#16813,
#16814,#16815,#16816,#16817,#16818,#16819,#16820,#16821,#16822,#16823,#16824,
#16825,#16826,#16827,#16828,#16829,#16830,#16831),(#16832,#16833,#16834,
#16835,#16836,#16837,#16838,#16839,#16840,#16841,#16842,#16843,#16844,#16845,
#16846,#16847,#16848,#16849,#16850,#16851,#16852,#16853,#16854,#16855,#16856,
#16857,#16858,#16859,#16860,#16861,#16862,#16863,#16864,#16865,#16866,#16867,
#16868,#16869,#16870,#16871,#16872,#16873,#16874,#16875,#16876,#16877,#16878,
#16879,#16880,#16881,#16882,#16883,#16884,#16885,#16886,#16887,#16888,#16889,
#16890,#16891,#16892,#16893,#16894,#16895,#16896,#16897,#16898,#16899,#16900,
#16901,#16902,#16903,#16904,#16905,#16906,#16907,#16908,#16909,#16910,#16911,
#16912,#16913,#16914,#16915,#16916,#16917,#16918,#16919,#16920,#16921,#16922,
#16923,#16924,#16925,#16926,#16927,#16928,#16929,#16930,#16931,#16932,#16933,
#16934,#16935,#16936,#16937,#16938,#16939,#16940,#16941,#16942,#16943,#16944,
#16945,#16946,#16947,#16948,#16949,#16950,#16951,#16952,#16953,#16954,#16955,
#16956,#16957,#16958),(#16959,#16960,#16961,#16962,#16963,#16964,#16965,
#16966,#16967,#16968,#16969,#16970,#16971,#16972,#16973,#16974,#16975,#16976,
#16977,#16978,#16979,#16980,#16981,#16982,#16983,#16984,#16985,#16986,#16987,
#16988,#16989,#16990,#16991,#16992,#16993,#16994,#16995,#16996,#16997,#16998,
#16999,#17000,#17001,#17002,#17003,#17004,#17005,#17006,#17007,#17008,#17009,
#17010,#17011,#17012,#17013,#17014,#17015,#17016,#17017,#17018,#17019,#17020,
#17021,#17022,#17023,#17024,#17025,#17026,#17027,#17028,#17029,#17030,#17031,
#17032,#17033,#17034,#17035,#17036,#17037,#17038,#17039,#17040,#17041,#17042,
#17043,#17044,#17045,#17046,#17047,#17048,#17049,#17050,#17051,#17052,#17053,
#17054,#17055,#17056,#17057,#17058,#17059,#17060,#17061,#17062,#17063,#17064,
#17065,#17066,#17067,#17068,#17069,#17070,#17071,#17072,#17073,#17074,#17075,
#17076,#17077,#17078,#17079,#17080,#17081,#17082,#17083,#17084,#17085),
(#17086,#17087,#17088,#17089,#17090,#17091,#17092,#17093,#17094,#17095,
#17096,#17097,#17098,#17099,#17100,#17101,#17102,#17103,#17104,#17105,#17106,
#17107,#17108,#17109,#17110,#17111,#17112,#17113,#17114,#17115,#17116,#17117,
#17118,#17119,#17120,#17121,#17122,#17123,#17124,#17125,#17126,#17127,#17128,
#17129,#17130,#17131,#17132,#17133,#17134,#17135,#17136,#17137,#17138,#17139,
#17140,#17141,#17142,#17143,#17144,#17145,#17146,#17147,#17148,#17149,#17150,
#17151,#17152,#17153,#17154,#17155,#17156,#17157,#17158,#17159,#17160,#17161,
#17162,#17163,#17164,#17165,#17166,#17167,#17168,#17169,#17170,#17171,#17172,
#17173,#17174,#17175,#17176,#17177,#17178,#17179,#17180,#17181,#17182,#17183,
#17184,#17185,#17186,#17187,#17188,#17189,#17190,#17191,#17192,#17193,#17194,
#17195,#17196,#17197,#17198,#17199,#17200,#17201,#17202,#17203,#17204,#17205,
#17206,#17207,#17208,#17209,#17210,#17211,#17212),(#17213,#17214,#17215,
#17216,#17217,#17218,#17219,#17220,#17221,#17222,#17223,#17224,#17225,#17226,
#17227,#17228,#17229,#17230,#17231,#17232,#17233,#17234,#17235,#17236,#17237,
#17238,#17239,#17240,#17241,#17242,#17243,#17244,#17245,#17246,#17247,#17248,
#17249,#17250,#17251,#17252,#17253,#17254,#17255,#17256,#17257,#17258,#17259,
#17260,#17261,#17262,#17263,#17264,#17265,#17266,#17267,#17268,#17269,#17270,
#17271,#17272,#17273,#17274,#17275,#17276,#17277,#17278,#17279,#17280,#17281,
#17282,#17283,#17284,#17285,#17286,#17287,#17288,#17289,#17290,#17291,#17292,
#17293,#17294,#17295,#17296,#17297,#17298,#17299,#17300,#17301,#17302,#17303,
#17304,#17305,#17306,#17307,#17308,#17309,#17310,#17311,#17312,#17313,#17314,
#17315,#17316,#17317,#17318,#17319,#17320,#17321,#17322,#17323,#17324,#17325,
#17326,#17327,#17328,#17329,#17330,#17331,#17332,#17333,#17334,#17335,#17336,
#17337,#17338,#17339),(#17340,#17341,#17342,#17343,#17344,#17345,#17346,
#17347,#17348,#17349,#17350,#17351,#17352,#17353,#17354,#17355,#17356,#17357,
#17358,#17359,#17360,#17361,#17362,#17363,#17364,#17365,#17366,#17367,#17368,
#17369,#17370,#17371,#17372,#17373,#17374,#17375,#17376,#17377,#17378,#17379,
#17380,#17381,#17382,#17383,#17384,#17385,#17386,#17387,#17388,#17389,#17390,
#17391,#17392,#17393,#17394,#17395,#17396,#17397,#17398,#17399,#17400,#17401,
#17402,#17403,#17404,#17405,#17406,#17407,#17408,#17409,#17410,#17411,#17412,
#17413,#17414,#17415,#17416,#17417,#17418,#17419,#17420,#17421,#17422,#17423,
#17424,#17425,#17426,#17427,#17428,#17429,#17430,#17431,#17432,#17433,#17434,
#17435,#17436,#17437,#17438,#17439,#17440,#17441,#17442,#17443,#17444,#17445,
#17446,#17447,#17448,#17449,#17450,#17451,#17452,#17453,#17454,#17455,#17456,
#17457,#17458,#17459,#17460,#17461,#17462,#17463,#17464,#17465,#17466)),
 .UNSPECIFIED.,.T.,.F.,.F.,(4,1,1,1,1,1,1,4),(4,1,1,1,1,1,1,1,1,1,1,1,1,
1,1,1,1,1,1,1,1,1,1,1,1,1,1,1,1,1,1,1,1,1,1,1,1,1,1,1,1,1,1,1,1,1,1,1,1,
1,1,1,1,1,1,1,1,1,1,1,1,1,1,1,1,1,1,1,1,1,1,1,1,1,1,1,1,1,1,1,1,1,1,1,1,
1,1,1,1,1,1,1,1,1,1,1,1,1,1,1,1,1,1,1,1,1,1,1,1,1,1,1,1,1,1,1,1,1,1,1,1,
1,1,1,4),(-3.14159265358979,-2.24399475256414,-1.34639685153848,-0.448798950512828,
0.448798950512828,1.34639685153848,2.24399475256414,3.14159265358979),(0.,
0.00892857142857143,0.0178571428571429,0.0267857142857143,0.0357142857142857,
0.0446428571428571,0.0535714285714286,0.0625,0.0714285714285714,0.0803571428571428,
0.0892857142857143,0.0982142857142857,0.107142857142857,0.116071428571429,
0.125,0.133928571428571,0.142857142857143,0.150793650793651,0.158730158730159,
0.166666666666667,0.174603174603175,0.182539682539683,0.19047619047619,
0.196428571428571,0.202380952380952,0.208333333333333,0.214285714285714,
0.222222222222222,0.23015873015873,0.238095238095238,0.244047619047619,
0.25,0.261904761904762,0.273809523809524,0.285714285714286,0.297619047619048,
0.30952380952381,0.321428571428571,0.333333333333333,0.337301587301587,
0.341269841269841,0.349206349206349,0.357142857142857,0.365079365079365,
0.373015873015873,0.380952380952381,0.386904761904762,0.392857142857143,
0.404761904761905,0.410714285714286,0.416666666666667,0.422619047619048,
0.428571428571429,0.4375,0.446428571428571,0.455357142857143,0.459821428571429,
0.464285714285714,0.470238095238095,0.476190476190476,0.482142857142857,
0.491071428571429,0.5,0.508928571428571,0.517857142857143,0.526785714285714,
0.535714285714286,0.544642857142857,0.553571428571429,0.5625,0.571428571428571,
0.580357142857143,0.589285714285714,0.598214285714286,0.607142857142857,
0.616071428571429,0.625,0.633928571428571,0.642857142857143,0.650793650793651,
0.658730158730159,0.666666666666667,0.672619047619048,0.678571428571428,
0.684523809523809,0.69047619047619,0.696428571428571,0.702380952380952,
0.708333333333333,0.714285714285714,0.720238095238095,0.726190476190476,
0.732142857142857,0.738095238095238,0.744047619047619,0.75,0.755952380952381,
0.761904761904762,0.76984126984127,0.777777777777778,0.785714285714286,
0.794642857142857,0.803571428571428,0.8125,0.821428571428571,0.830357142857143,
0.839285714285714,0.848214285714286,0.857142857142857,0.866071428571429,
0.875,0.883928571428571,0.892857142857143,0.901785714285714,0.910714285714286,
0.919642857142857,0.928571428571429,0.9375,0.946428571428571,0.955357142857143,
0.964285714285714,0.973214285714286,0.982142857142857,0.991071428571429,
1.),.UNSPECIFIED.);
#592=B_SPLINE_SURFACE_WITH_KNOTS('',3,3,((#17754,#17755,#17756,#17757,#17758,
#17759,#17760,#17761,#17762,#17763,#17764,#17765,#17766,#17767,#17768,#17769,
#17770,#17771,#17772,#17773,#17774,#17775,#17776,#17777,#17778,#17779,#17780,
#17781,#17782,#17783,#17784,#17785,#17786,#17787,#17788,#17789,#17790,#17791,
#17792,#17793,#17794,#17795,#17796,#17797,#17798,#17799,#17800,#17801,#17802,
#17803,#17804,#17805,#17806,#17807,#17808,#17809,#17810,#17811,#17812,#17813,
#17814,#17815,#17816,#17817,#17818,#17819,#17820,#17821,#17822,#17823,#17824,
#17825,#17826,#17827,#17828,#17829,#17830,#17831,#17832,#17833,#17834,#17835,
#17836,#17837,#17838,#17839,#17840,#17841,#17842,#17843,#17844,#17845,#17846,
#17847,#17848,#17849,#17850,#17851,#17852,#17853,#17854,#17855,#17856,#17857,
#17858,#17859,#17860,#17861,#17862,#17863,#17864,#17865,#17866,#17867,#17868,
#17869,#17870,#17871,#17872,#17873,#17874,#17875,#17876,#17877,#17878,#17879,
#17880,#17881,#17882,#17883,#17884,#17885,#17886,#17887,#17888,#17889,#17890,
#17891),(#17892,#17893,#17894,#17895,#17896,#17897,#17898,#17899,#17900,
#17901,#17902,#17903,#17904,#17905,#17906,#17907,#17908,#17909,#17910,#17911,
#17912,#17913,#17914,#17915,#17916,#17917,#17918,#17919,#17920,#17921,#17922,
#17923,#17924,#17925,#17926,#17927,#17928,#17929,#17930,#17931,#17932,#17933,
#17934,#17935,#17936,#17937,#17938,#17939,#17940,#17941,#17942,#17943,#17944,
#17945,#17946,#17947,#17948,#17949,#17950,#17951,#17952,#17953,#17954,#17955,
#17956,#17957,#17958,#17959,#17960,#17961,#17962,#17963,#17964,#17965,#17966,
#17967,#17968,#17969,#17970,#17971,#17972,#17973,#17974,#17975,#17976,#17977,
#17978,#17979,#17980,#17981,#17982,#17983,#17984,#17985,#17986,#17987,#17988,
#17989,#17990,#17991,#17992,#17993,#17994,#17995,#17996,#17997,#17998,#17999,
#18000,#18001,#18002,#18003,#18004,#18005,#18006,#18007,#18008,#18009,#18010,
#18011,#18012,#18013,#18014,#18015,#18016,#18017,#18018,#18019,#18020,#18021,
#18022,#18023,#18024,#18025,#18026,#18027,#18028,#18029),(#18030,#18031,
#18032,#18033,#18034,#18035,#18036,#18037,#18038,#18039,#18040,#18041,#18042,
#18043,#18044,#18045,#18046,#18047,#18048,#18049,#18050,#18051,#18052,#18053,
#18054,#18055,#18056,#18057,#18058,#18059,#18060,#18061,#18062,#18063,#18064,
#18065,#18066,#18067,#18068,#18069,#18070,#18071,#18072,#18073,#18074,#18075,
#18076,#18077,#18078,#18079,#18080,#18081,#18082,#18083,#18084,#18085,#18086,
#18087,#18088,#18089,#18090,#18091,#18092,#18093,#18094,#18095,#18096,#18097,
#18098,#18099,#18100,#18101,#18102,#18103,#18104,#18105,#18106,#18107,#18108,
#18109,#18110,#18111,#18112,#18113,#18114,#18115,#18116,#18117,#18118,#18119,
#18120,#18121,#18122,#18123,#18124,#18125,#18126,#18127,#18128,#18129,#18130,
#18131,#18132,#18133,#18134,#18135,#18136,#18137,#18138,#18139,#18140,#18141,
#18142,#18143,#18144,#18145,#18146,#18147,#18148,#18149,#18150,#18151,#18152,
#18153,#18154,#18155,#18156,#18157,#18158,#18159,#18160,#18161,#18162,#18163,
#18164,#18165,#18166,#18167),(#18168,#18169,#18170,#18171,#18172,#18173,
#18174,#18175,#18176,#18177,#18178,#18179,#18180,#18181,#18182,#18183,#18184,
#18185,#18186,#18187,#18188,#18189,#18190,#18191,#18192,#18193,#18194,#18195,
#18196,#18197,#18198,#18199,#18200,#18201,#18202,#18203,#18204,#18205,#18206,
#18207,#18208,#18209,#18210,#18211,#18212,#18213,#18214,#18215,#18216,#18217,
#18218,#18219,#18220,#18221,#18222,#18223,#18224,#18225,#18226,#18227,#18228,
#18229,#18230,#18231,#18232,#18233,#18234,#18235,#18236,#18237,#18238,#18239,
#18240,#18241,#18242,#18243,#18244,#18245,#18246,#18247,#18248,#18249,#18250,
#18251,#18252,#18253,#18254,#18255,#18256,#18257,#18258,#18259,#18260,#18261,
#18262,#18263,#18264,#18265,#18266,#18267,#18268,#18269,#18270,#18271,#18272,
#18273,#18274,#18275,#18276,#18277,#18278,#18279,#18280,#18281,#18282,#18283,
#18284,#18285,#18286,#18287,#18288,#18289,#18290,#18291,#18292,#18293,#18294,
#18295,#18296,#18297,#18298,#18299,#18300,#18301,#18302,#18303,#18304,#18305),
(#18306,#18307,#18308,#18309,#18310,#18311,#18312,#18313,#18314,#18315,
#18316,#18317,#18318,#18319,#18320,#18321,#18322,#18323,#18324,#18325,#18326,
#18327,#18328,#18329,#18330,#18331,#18332,#18333,#18334,#18335,#18336,#18337,
#18338,#18339,#18340,#18341,#18342,#18343,#18344,#18345,#18346,#18347,#18348,
#18349,#18350,#18351,#18352,#18353,#18354,#18355,#18356,#18357,#18358,#18359,
#18360,#18361,#18362,#18363,#18364,#18365,#18366,#18367,#18368,#18369,#18370,
#18371,#18372,#18373,#18374,#18375,#18376,#18377,#18378,#18379,#18380,#18381,
#18382,#18383,#18384,#18385,#18386,#18387,#18388,#18389,#18390,#18391,#18392,
#18393,#18394,#18395,#18396,#18397,#18398,#18399,#18400,#18401,#18402,#18403,
#18404,#18405,#18406,#18407,#18408,#18409,#18410,#18411,#18412,#18413,#18414,
#18415,#18416,#18417,#18418,#18419,#18420,#18421,#18422,#18423,#18424,#18425,
#18426,#18427,#18428,#18429,#18430,#18431,#18432,#18433,#18434,#18435,#18436,
#18437,#18438,#18439,#18440,#18441,#18442,#18443),(#18444,#18445,#18446,
#18447,#18448,#18449,#18450,#18451,#18452,#18453,#18454,#18455,#18456,#18457,
#18458,#18459,#18460,#18461,#18462,#18463,#18464,#18465,#18466,#18467,#18468,
#18469,#18470,#18471,#18472,#18473,#18474,#18475,#18476,#18477,#18478,#18479,
#18480,#18481,#18482,#18483,#18484,#18485,#18486,#18487,#18488,#18489,#18490,
#18491,#18492,#18493,#18494,#18495,#18496,#18497,#18498,#18499,#18500,#18501,
#18502,#18503,#18504,#18505,#18506,#18507,#18508,#18509,#18510,#18511,#18512,
#18513,#18514,#18515,#18516,#18517,#18518,#18519,#18520,#18521,#18522,#18523,
#18524,#18525,#18526,#18527,#18528,#18529,#18530,#18531,#18532,#18533,#18534,
#18535,#18536,#18537,#18538,#18539,#18540,#18541,#18542,#18543,#18544,#18545,
#18546,#18547,#18548,#18549,#18550,#18551,#18552,#18553,#18554,#18555,#18556,
#18557,#18558,#18559,#18560,#18561,#18562,#18563,#18564,#18565,#18566,#18567,
#18568,#18569,#18570,#18571,#18572,#18573,#18574,#18575,#18576,#18577,#18578,
#18579,#18580,#18581),(#18582,#18583,#18584,#18585,#18586,#18587,#18588,
#18589,#18590,#18591,#18592,#18593,#18594,#18595,#18596,#18597,#18598,#18599,
#18600,#18601,#18602,#18603,#18604,#18605,#18606,#18607,#18608,#18609,#18610,
#18611,#18612,#18613,#18614,#18615,#18616,#18617,#18618,#18619,#18620,#18621,
#18622,#18623,#18624,#18625,#18626,#18627,#18628,#18629,#18630,#18631,#18632,
#18633,#18634,#18635,#18636,#18637,#18638,#18639,#18640,#18641,#18642,#18643,
#18644,#18645,#18646,#18647,#18648,#18649,#18650,#18651,#18652,#18653,#18654,
#18655,#18656,#18657,#18658,#18659,#18660,#18661,#18662,#18663,#18664,#18665,
#18666,#18667,#18668,#18669,#18670,#18671,#18672,#18673,#18674,#18675,#18676,
#18677,#18678,#18679,#18680,#18681,#18682,#18683,#18684,#18685,#18686,#18687,
#18688,#18689,#18690,#18691,#18692,#18693,#18694,#18695,#18696,#18697,#18698,
#18699,#18700,#18701,#18702,#18703,#18704,#18705,#18706,#18707,#18708,#18709,
#18710,#18711,#18712,#18713,#18714,#18715,#18716,#18717,#18718,#18719),
(#18720,#18721,#18722,#18723,#18724,#18725,#18726,#18727,#18728,#18729,
#18730,#18731,#18732,#18733,#18734,#18735,#18736,#18737,#18738,#18739,#18740,
#18741,#18742,#18743,#18744,#18745,#18746,#18747,#18748,#18749,#18750,#18751,
#18752,#18753,#18754,#18755,#18756,#18757,#18758,#18759,#18760,#18761,#18762,
#18763,#18764,#18765,#18766,#18767,#18768,#18769,#18770,#18771,#18772,#18773,
#18774,#18775,#18776,#18777,#18778,#18779,#18780,#18781,#18782,#18783,#18784,
#18785,#18786,#18787,#18788,#18789,#18790,#18791,#18792,#18793,#18794,#18795,
#18796,#18797,#18798,#18799,#18800,#18801,#18802,#18803,#18804,#18805,#18806,
#18807,#18808,#18809,#18810,#18811,#18812,#18813,#18814,#18815,#18816,#18817,
#18818,#18819,#18820,#18821,#18822,#18823,#18824,#18825,#18826,#18827,#18828,
#18829,#18830,#18831,#18832,#18833,#18834,#18835,#18836,#18837,#18838,#18839,
#18840,#18841,#18842,#18843,#18844,#18845,#18846,#18847,#18848,#18849,#18850,
#18851,#18852,#18853,#18854,#18855,#18856,#18857),(#18858,#18859,#18860,
#18861,#18862,#18863,#18864,#18865,#18866,#18867,#18868,#18869,#18870,#18871,
#18872,#18873,#18874,#18875,#18876,#18877,#18878,#18879,#18880,#18881,#18882,
#18883,#18884,#18885,#18886,#18887,#18888,#18889,#18890,#18891,#18892,#18893,
#18894,#18895,#18896,#18897,#18898,#18899,#18900,#18901,#18902,#18903,#18904,
#18905,#18906,#18907,#18908,#18909,#18910,#18911,#18912,#18913,#18914,#18915,
#18916,#18917,#18918,#18919,#18920,#18921,#18922,#18923,#18924,#18925,#18926,
#18927,#18928,#18929,#18930,#18931,#18932,#18933,#18934,#18935,#18936,#18937,
#18938,#18939,#18940,#18941,#18942,#18943,#18944,#18945,#18946,#18947,#18948,
#18949,#18950,#18951,#18952,#18953,#18954,#18955,#18956,#18957,#18958,#18959,
#18960,#18961,#18962,#18963,#18964,#18965,#18966,#18967,#18968,#18969,#18970,
#18971,#18972,#18973,#18974,#18975,#18976,#18977,#18978,#18979,#18980,#18981,
#18982,#18983,#18984,#18985,#18986,#18987,#18988,#18989,#18990,#18991,#18992,
#18993,#18994,#18995),(#18996,#18997,#18998,#18999,#19000,#19001,#19002,
#19003,#19004,#19005,#19006,#19007,#19008,#19009,#19010,#19011,#19012,#19013,
#19014,#19015,#19016,#19017,#19018,#19019,#19020,#19021,#19022,#19023,#19024,
#19025,#19026,#19027,#19028,#19029,#19030,#19031,#19032,#19033,#19034,#19035,
#19036,#19037,#19038,#19039,#19040,#19041,#19042,#19043,#19044,#19045,#19046,
#19047,#19048,#19049,#19050,#19051,#19052,#19053,#19054,#19055,#19056,#19057,
#19058,#19059,#19060,#19061,#19062,#19063,#19064,#19065,#19066,#19067,#19068,
#19069,#19070,#19071,#19072,#19073,#19074,#19075,#19076,#19077,#19078,#19079,
#19080,#19081,#19082,#19083,#19084,#19085,#19086,#19087,#19088,#19089,#19090,
#19091,#19092,#19093,#19094,#19095,#19096,#19097,#19098,#19099,#19100,#19101,
#19102,#19103,#19104,#19105,#19106,#19107,#19108,#19109,#19110,#19111,#19112,
#19113,#19114,#19115,#19116,#19117,#19118,#19119,#19120,#19121,#19122,#19123,
#19124,#19125,#19126,#19127,#19128,#19129,#19130,#19131,#19132,#19133)),
 .UNSPECIFIED.,.T.,.F.,.F.,(4,1,1,1,1,1,1,4),(4,1,1,1,1,1,1,1,1,1,1,1,1,
1,1,1,1,1,1,1,1,1,1,1,1,1,1,1,1,1,1,1,1,1,1,1,1,1,1,1,1,1,1,1,1,1,1,1,1,
1,1,1,1,1,1,1,1,1,1,1,1,1,1,1,1,1,1,1,1,1,1,1,1,1,1,1,1,1,1,1,1,1,1,1,1,
1,1,1,1,1,1,1,1,1,1,1,1,1,1,1,1,1,1,1,1,1,1,1,1,1,1,1,1,1,1,1,1,1,1,1,1,
1,1,1,1,1,1,1,1,1,1,1,1,1,1,4),(-3.14159265358979,-2.24399475256414,-1.34639685153848,
-0.448798950512828,0.448798950512828,1.34639685153848,2.24399475256414,
3.14159265358979),(0.,0.00892857142857143,0.0178571428571429,0.0267857142857143,
0.0357142857142857,0.0446428571428571,0.0535714285714286,0.0625,0.0714285714285714,
0.0803571428571428,0.0892857142857143,0.0982142857142857,0.107142857142857,
0.116071428571429,0.125,0.133928571428571,0.142857142857143,0.150793650793651,
0.154761904761905,0.156746031746032,0.158730158730159,0.166666666666667,
0.174603174603175,0.182539682539683,0.19047619047619,0.196428571428571,
0.202380952380952,0.208333333333333,0.214285714285714,0.222222222222222,
0.23015873015873,0.238095238095238,0.241071428571429,0.244047619047619,
0.25,0.255952380952381,0.261904761904762,0.267857142857143,0.273809523809524,
0.279761904761905,0.285714285714286,0.297619047619048,0.30952380952381,
0.321428571428571,0.327380952380952,0.333333333333333,0.341269841269841,
0.349206349206349,0.357142857142857,0.361111111111111,0.363095238095238,
0.365079365079365,0.373015873015873,0.380952380952381,0.386904761904762,
0.392857142857143,0.398809523809524,0.404761904761905,0.410714285714286,
0.416666666666667,0.422619047619048,0.428571428571429,0.4375,0.446428571428571,
0.455357142857143,0.459821428571429,0.464285714285714,0.470238095238095,
0.476190476190476,0.482142857142857,0.491071428571429,0.5,0.508928571428571,
0.517857142857143,0.526785714285714,0.535714285714286,0.544642857142857,
0.553571428571429,0.5625,0.571428571428571,0.580357142857143,0.589285714285714,
0.598214285714286,0.607142857142857,0.616071428571429,0.625,0.633928571428571,
0.642857142857143,0.650793650793651,0.658730158730159,0.666666666666667,
0.672619047619048,0.678571428571428,0.684523809523809,0.69047619047619,
0.696428571428571,0.702380952380952,0.708333333333333,0.714285714285714,
0.720238095238095,0.726190476190476,0.732142857142857,0.738095238095238,
0.744047619047619,0.75,0.755952380952381,0.761904761904762,0.76984126984127,
0.777777777777778,0.785714285714286,0.787946428571428,0.790178571428571,
0.794642857142857,0.803571428571428,0.8125,0.821428571428571,0.830357142857143,
0.839285714285714,0.848214285714286,0.857142857142857,0.866071428571429,
0.875,0.883928571428571,0.892857142857143,0.901785714285714,0.910714285714286,
0.919642857142857,0.928571428571429,0.9375,0.946428571428571,0.955357142857143,
0.964285714285714,0.973214285714286,0.982142857142857,0.991071428571429,
1.),.UNSPECIFIED.);
#593=B_SPLINE_SURFACE_WITH_KNOTS('',3,3,((#19432,#19433,#19434,#19435,#19436,
#19437,#19438,#19439,#19440,#19441,#19442,#19443,#19444,#19445,#19446,#19447,
#19448,#19449,#19450,#19451,#19452,#19453,#19454,#19455,#19456,#19457,#19458,
#19459,#19460,#19461,#19462,#19463,#19464,#19465,#19466,#19467,#19468,#19469,
#19470,#19471,#19472,#19473,#19474,#19475,#19476,#19477,#19478,#19479,#19480,
#19481,#19482,#19483,#19484,#19485,#19486,#19487,#19488,#19489,#19490,#19491,
#19492,#19493,#19494,#19495,#19496,#19497,#19498,#19499,#19500,#19501,#19502,
#19503,#19504,#19505,#19506,#19507,#19508,#19509,#19510,#19511,#19512,#19513,
#19514,#19515,#19516,#19517,#19518,#19519,#19520,#19521,#19522,#19523,#19524,
#19525,#19526,#19527,#19528,#19529,#19530,#19531,#19532,#19533,#19534,#19535,
#19536,#19537,#19538,#19539,#19540,#19541,#19542,#19543,#19544,#19545,#19546,
#19547,#19548,#19549,#19550,#19551,#19552,#19553,#19554,#19555,#19556,#19557,
#19558),(#19559,#19560,#19561,#19562,#19563,#19564,#19565,#19566,#19567,
#19568,#19569,#19570,#19571,#19572,#19573,#19574,#19575,#19576,#19577,#19578,
#19579,#19580,#19581,#19582,#19583,#19584,#19585,#19586,#19587,#19588,#19589,
#19590,#19591,#19592,#19593,#19594,#19595,#19596,#19597,#19598,#19599,#19600,
#19601,#19602,#19603,#19604,#19605,#19606,#19607,#19608,#19609,#19610,#19611,
#19612,#19613,#19614,#19615,#19616,#19617,#19618,#19619,#19620,#19621,#19622,
#19623,#19624,#19625,#19626,#19627,#19628,#19629,#19630,#19631,#19632,#19633,
#19634,#19635,#19636,#19637,#19638,#19639,#19640,#19641,#19642,#19643,#19644,
#19645,#19646,#19647,#19648,#19649,#19650,#19651,#19652,#19653,#19654,#19655,
#19656,#19657,#19658,#19659,#19660,#19661,#19662,#19663,#19664,#19665,#19666,
#19667,#19668,#19669,#19670,#19671,#19672,#19673,#19674,#19675,#19676,#19677,
#19678,#19679,#19680,#19681,#19682,#19683,#19684,#19685),(#19686,#19687,
#19688,#19689,#19690,#19691,#19692,#19693,#19694,#19695,#19696,#19697,#19698,
#19699,#19700,#19701,#19702,#19703,#19704,#19705,#19706,#19707,#19708,#19709,
#19710,#19711,#19712,#19713,#19714,#19715,#19716,#19717,#19718,#19719,#19720,
#19721,#19722,#19723,#19724,#19725,#19726,#19727,#19728,#19729,#19730,#19731,
#19732,#19733,#19734,#19735,#19736,#19737,#19738,#19739,#19740,#19741,#19742,
#19743,#19744,#19745,#19746,#19747,#19748,#19749,#19750,#19751,#19752,#19753,
#19754,#19755,#19756,#19757,#19758,#19759,#19760,#19761,#19762,#19763,#19764,
#19765,#19766,#19767,#19768,#19769,#19770,#19771,#19772,#19773,#19774,#19775,
#19776,#19777,#19778,#19779,#19780,#19781,#19782,#19783,#19784,#19785,#19786,
#19787,#19788,#19789,#19790,#19791,#19792,#19793,#19794,#19795,#19796,#19797,
#19798,#19799,#19800,#19801,#19802,#19803,#19804,#19805,#19806,#19807,#19808,
#19809,#19810,#19811,#19812),(#19813,#19814,#19815,#19816,#19817,#19818,
#19819,#19820,#19821,#19822,#19823,#19824,#19825,#19826,#19827,#19828,#19829,
#19830,#19831,#19832,#19833,#19834,#19835,#19836,#19837,#19838,#19839,#19840,
#19841,#19842,#19843,#19844,#19845,#19846,#19847,#19848,#19849,#19850,#19851,
#19852,#19853,#19854,#19855,#19856,#19857,#19858,#19859,#19860,#19861,#19862,
#19863,#19864,#19865,#19866,#19867,#19868,#19869,#19870,#19871,#19872,#19873,
#19874,#19875,#19876,#19877,#19878,#19879,#19880,#19881,#19882,#19883,#19884,
#19885,#19886,#19887,#19888,#19889,#19890,#19891,#19892,#19893,#19894,#19895,
#19896,#19897,#19898,#19899,#19900,#19901,#19902,#19903,#19904,#19905,#19906,
#19907,#19908,#19909,#19910,#19911,#19912,#19913,#19914,#19915,#19916,#19917,
#19918,#19919,#19920,#19921,#19922,#19923,#19924,#19925,#19926,#19927,#19928,
#19929,#19930,#19931,#19932,#19933,#19934,#19935,#19936,#19937,#19938,#19939),
(#19940,#19941,#19942,#19943,#19944,#19945,#19946,#19947,#19948,#19949,
#19950,#19951,#19952,#19953,#19954,#19955,#19956,#19957,#19958,#19959,#19960,
#19961,#19962,#19963,#19964,#19965,#19966,#19967,#19968,#19969,#19970,#19971,
#19972,#19973,#19974,#19975,#19976,#19977,#19978,#19979,#19980,#19981,#19982,
#19983,#19984,#19985,#19986,#19987,#19988,#19989,#19990,#19991,#19992,#19993,
#19994,#19995,#19996,#19997,#19998,#19999,#20000,#20001,#20002,#20003,#20004,
#20005,#20006,#20007,#20008,#20009,#20010,#20011,#20012,#20013,#20014,#20015,
#20016,#20017,#20018,#20019,#20020,#20021,#20022,#20023,#20024,#20025,#20026,
#20027,#20028,#20029,#20030,#20031,#20032,#20033,#20034,#20035,#20036,#20037,
#20038,#20039,#20040,#20041,#20042,#20043,#20044,#20045,#20046,#20047,#20048,
#20049,#20050,#20051,#20052,#20053,#20054,#20055,#20056,#20057,#20058,#20059,
#20060,#20061,#20062,#20063,#20064,#20065,#20066),(#20067,#20068,#20069,
#20070,#20071,#20072,#20073,#20074,#20075,#20076,#20077,#20078,#20079,#20080,
#20081,#20082,#20083,#20084,#20085,#20086,#20087,#20088,#20089,#20090,#20091,
#20092,#20093,#20094,#20095,#20096,#20097,#20098,#20099,#20100,#20101,#20102,
#20103,#20104,#20105,#20106,#20107,#20108,#20109,#20110,#20111,#20112,#20113,
#20114,#20115,#20116,#20117,#20118,#20119,#20120,#20121,#20122,#20123,#20124,
#20125,#20126,#20127,#20128,#20129,#20130,#20131,#20132,#20133,#20134,#20135,
#20136,#20137,#20138,#20139,#20140,#20141,#20142,#20143,#20144,#20145,#20146,
#20147,#20148,#20149,#20150,#20151,#20152,#20153,#20154,#20155,#20156,#20157,
#20158,#20159,#20160,#20161,#20162,#20163,#20164,#20165,#20166,#20167,#20168,
#20169,#20170,#20171,#20172,#20173,#20174,#20175,#20176,#20177,#20178,#20179,
#20180,#20181,#20182,#20183,#20184,#20185,#20186,#20187,#20188,#20189,#20190,
#20191,#20192,#20193),(#20194,#20195,#20196,#20197,#20198,#20199,#20200,
#20201,#20202,#20203,#20204,#20205,#20206,#20207,#20208,#20209,#20210,#20211,
#20212,#20213,#20214,#20215,#20216,#20217,#20218,#20219,#20220,#20221,#20222,
#20223,#20224,#20225,#20226,#20227,#20228,#20229,#20230,#20231,#20232,#20233,
#20234,#20235,#20236,#20237,#20238,#20239,#20240,#20241,#20242,#20243,#20244,
#20245,#20246,#20247,#20248,#20249,#20250,#20251,#20252,#20253,#20254,#20255,
#20256,#20257,#20258,#20259,#20260,#20261,#20262,#20263,#20264,#20265,#20266,
#20267,#20268,#20269,#20270,#20271,#20272,#20273,#20274,#20275,#20276,#20277,
#20278,#20279,#20280,#20281,#20282,#20283,#20284,#20285,#20286,#20287,#20288,
#20289,#20290,#20291,#20292,#20293,#20294,#20295,#20296,#20297,#20298,#20299,
#20300,#20301,#20302,#20303,#20304,#20305,#20306,#20307,#20308,#20309,#20310,
#20311,#20312,#20313,#20314,#20315,#20316,#20317,#20318,#20319,#20320),
(#20321,#20322,#20323,#20324,#20325,#20326,#20327,#20328,#20329,#20330,
#20331,#20332,#20333,#20334,#20335,#20336,#20337,#20338,#20339,#20340,#20341,
#20342,#20343,#20344,#20345,#20346,#20347,#20348,#20349,#20350,#20351,#20352,
#20353,#20354,#20355,#20356,#20357,#20358,#20359,#20360,#20361,#20362,#20363,
#20364,#20365,#20366,#20367,#20368,#20369,#20370,#20371,#20372,#20373,#20374,
#20375,#20376,#20377,#20378,#20379,#20380,#20381,#20382,#20383,#20384,#20385,
#20386,#20387,#20388,#20389,#20390,#20391,#20392,#20393,#20394,#20395,#20396,
#20397,#20398,#20399,#20400,#20401,#20402,#20403,#20404,#20405,#20406,#20407,
#20408,#20409,#20410,#20411,#20412,#20413,#20414,#20415,#20416,#20417,#20418,
#20419,#20420,#20421,#20422,#20423,#20424,#20425,#20426,#20427,#20428,#20429,
#20430,#20431,#20432,#20433,#20434,#20435,#20436,#20437,#20438,#20439,#20440,
#20441,#20442,#20443,#20444,#20445,#20446,#20447),(#20448,#20449,#20450,
#20451,#20452,#20453,#20454,#20455,#20456,#20457,#20458,#20459,#20460,#20461,
#20462,#20463,#20464,#20465,#20466,#20467,#20468,#20469,#20470,#20471,#20472,
#20473,#20474,#20475,#20476,#20477,#20478,#20479,#20480,#20481,#20482,#20483,
#20484,#20485,#20486,#20487,#20488,#20489,#20490,#20491,#20492,#20493,#20494,
#20495,#20496,#20497,#20498,#20499,#20500,#20501,#20502,#20503,#20504,#20505,
#20506,#20507,#20508,#20509,#20510,#20511,#20512,#20513,#20514,#20515,#20516,
#20517,#20518,#20519,#20520,#20521,#20522,#20523,#20524,#20525,#20526,#20527,
#20528,#20529,#20530,#20531,#20532,#20533,#20534,#20535,#20536,#20537,#20538,
#20539,#20540,#20541,#20542,#20543,#20544,#20545,#20546,#20547,#20548,#20549,
#20550,#20551,#20552,#20553,#20554,#20555,#20556,#20557,#20558,#20559,#20560,
#20561,#20562,#20563,#20564,#20565,#20566,#20567,#20568,#20569,#20570,#20571,
#20572,#20573,#20574),(#20575,#20576,#20577,#20578,#20579,#20580,#20581,
#20582,#20583,#20584,#20585,#20586,#20587,#20588,#20589,#20590,#20591,#20592,
#20593,#20594,#20595,#20596,#20597,#20598,#20599,#20600,#20601,#20602,#20603,
#20604,#20605,#20606,#20607,#20608,#20609,#20610,#20611,#20612,#20613,#20614,
#20615,#20616,#20617,#20618,#20619,#20620,#20621,#20622,#20623,#20624,#20625,
#20626,#20627,#20628,#20629,#20630,#20631,#20632,#20633,#20634,#20635,#20636,
#20637,#20638,#20639,#20640,#20641,#20642,#20643,#20644,#20645,#20646,#20647,
#20648,#20649,#20650,#20651,#20652,#20653,#20654,#20655,#20656,#20657,#20658,
#20659,#20660,#20661,#20662,#20663,#20664,#20665,#20666,#20667,#20668,#20669,
#20670,#20671,#20672,#20673,#20674,#20675,#20676,#20677,#20678,#20679,#20680,
#20681,#20682,#20683,#20684,#20685,#20686,#20687,#20688,#20689,#20690,#20691,
#20692,#20693,#20694,#20695,#20696,#20697,#20698,#20699,#20700,#20701)),
 .UNSPECIFIED.,.T.,.F.,.F.,(4,1,1,1,1,1,1,4),(4,1,1,1,1,1,1,1,1,1,1,1,1,
1,1,1,1,1,1,1,1,1,1,1,1,1,1,1,1,1,1,1,1,1,1,1,1,1,1,1,1,1,1,1,1,1,1,1,1,
1,1,1,1,1,1,1,1,1,1,1,1,1,1,1,1,1,1,1,1,1,1,1,1,1,1,1,1,1,1,1,1,1,1,1,1,
1,1,1,1,1,1,1,1,1,1,1,1,1,1,1,1,1,1,1,1,1,1,1,1,1,1,1,1,1,1,1,1,1,1,1,1,
1,1,1,4),(-3.14159265358979,-2.24399475256414,-1.34639685153848,-0.448798950512828,
0.448798950512828,1.34639685153848,2.24399475256414,3.14159265358979),(0.,
0.00892857142857143,0.0178571428571429,0.0267857142857143,0.0357142857142857,
0.0446428571428571,0.0535714285714286,0.0625,0.0714285714285714,0.0803571428571428,
0.0892857142857143,0.0982142857142857,0.107142857142857,0.116071428571429,
0.125,0.133928571428571,0.142857142857143,0.150793650793651,0.158730158730159,
0.166666666666667,0.174603174603175,0.182539682539683,0.19047619047619,
0.196428571428571,0.202380952380952,0.208333333333333,0.214285714285714,
0.222222222222222,0.23015873015873,0.238095238095238,0.244047619047619,
0.25,0.261904761904762,0.273809523809524,0.285714285714286,0.297619047619048,
0.30952380952381,0.321428571428571,0.333333333333333,0.337301587301587,
0.341269841269841,0.349206349206349,0.357142857142857,0.365079365079365,
0.373015873015873,0.380952380952381,0.386904761904762,0.392857142857143,
0.404761904761905,0.410714285714286,0.416666666666667,0.422619047619048,
0.428571428571429,0.4375,0.446428571428571,0.455357142857143,0.459821428571429,
0.464285714285714,0.470238095238095,0.476190476190476,0.482142857142857,
0.491071428571429,0.5,0.508928571428571,0.517857142857143,0.526785714285714,
0.535714285714286,0.544642857142857,0.553571428571429,0.5625,0.571428571428571,
0.580357142857143,0.589285714285714,0.598214285714286,0.607142857142857,
0.616071428571429,0.625,0.633928571428571,0.642857142857143,0.650793650793651,
0.658730158730159,0.666666666666667,0.672619047619048,0.678571428571428,
0.684523809523809,0.69047619047619,0.696428571428571,0.702380952380952,
0.708333333333333,0.714285714285714,0.720238095238095,0.726190476190476,
0.732142857142857,0.738095238095238,0.744047619047619,0.75,0.755952380952381,
0.761904761904762,0.76984126984127,0.777777777777778,0.785714285714286,
0.794642857142857,0.803571428571428,0.8125,0.821428571428571,0.830357142857143,
0.839285714285714,0.848214285714286,0.857142857142857,0.866071428571429,
0.875,0.883928571428571,0.892857142857143,0.901785714285714,0.910714285714286,
0.919642857142857,0.928571428571429,0.9375,0.946428571428571,0.955357142857143,
0.964285714285714,0.973214285714286,0.982142857142857,0.991071428571429,
1.),.UNSPECIFIED.);
#594=SHAPE_REPRESENTATION_RELATIONSHIP('SRR','None',#22640,#640);
#595=SHAPE_REPRESENTATION_RELATIONSHIP('SRR','None',#22641,#641);
#596=SHAPE_REPRESENTATION_RELATIONSHIP('SRR','None',#22642,#642);
#597=SHAPE_REPRESENTATION_RELATIONSHIP('SRR','None',#22643,#643);
#598=SHAPE_REPRESENTATION_RELATIONSHIP('SRR','None',#22644,#644);
#599=SHAPE_REPRESENTATION_RELATIONSHIP('SRR','None',#22645,#645);
#600=SHAPE_REPRESENTATION_RELATIONSHIP('SRR','None',#22646,#646);
#601=SHAPE_REPRESENTATION_RELATIONSHIP('SRR','None',#22647,#647);
#602=SHAPE_REPRESENTATION_RELATIONSHIP('SRR','None',#22648,#648);
#603=SHAPE_REPRESENTATION_RELATIONSHIP('SRR','None',#22649,#649);
#604=SHAPE_REPRESENTATION_RELATIONSHIP('SRR','None',#22650,#650);
#605=SHAPE_REPRESENTATION_RELATIONSHIP('SRR','None',#22651,#651);
#606=SHAPE_REPRESENTATION_RELATIONSHIP('SRR','None',#22652,#652);
#607=SHAPE_REPRESENTATION_RELATIONSHIP('SRR','None',#22653,#653);
#608=SHAPE_REPRESENTATION_RELATIONSHIP('SRR','None',#22654,#654);
#609=SHAPE_REPRESENTATION_RELATIONSHIP('SRR','None',#22655,#655);
#610=SHAPE_REPRESENTATION_RELATIONSHIP('SRR','None',#22656,#656);
#611=SHAPE_REPRESENTATION_RELATIONSHIP('SRR','None',#22657,#657);
#612=SHAPE_REPRESENTATION_RELATIONSHIP('SRR','None',#22658,#658);
#613=SHAPE_REPRESENTATION_RELATIONSHIP('SRR','None',#22659,#659);
#614=SHAPE_REPRESENTATION_RELATIONSHIP('SRR','None',#22660,#660);
#615=SHAPE_REPRESENTATION_RELATIONSHIP('SRR','None',#22661,#661);
#616=SHAPE_REPRESENTATION_RELATIONSHIP('SRR','None',#22662,#662);
#617=SHAPE_REPRESENTATION_RELATIONSHIP('SRR','None',#22663,#663);
#618=SHAPE_REPRESENTATION_RELATIONSHIP('SRR','None',#22664,#664);
#619=SHAPE_REPRESENTATION_RELATIONSHIP('SRR','None',#22665,#665);
#620=SHAPE_REPRESENTATION_RELATIONSHIP('SRR','None',#22666,#666);
#621=SHAPE_REPRESENTATION_RELATIONSHIP('SRR','None',#22667,#667);
#622=SHAPE_REPRESENTATION_RELATIONSHIP('SRR','None',#22668,#668);
#623=SHAPE_REPRESENTATION_RELATIONSHIP('SRR','None',#22669,#669);
#624=SHAPE_REPRESENTATION_RELATIONSHIP('SRR','None',#22670,#670);
#625=SHAPE_REPRESENTATION_RELATIONSHIP('SRR','None',#22671,#671);
#626=SHAPE_REPRESENTATION_RELATIONSHIP('SRR','None',#22672,#672);
#627=SHAPE_REPRESENTATION_RELATIONSHIP('SRR','None',#22673,#673);
#628=SHAPE_REPRESENTATION_RELATIONSHIP('SRR','None',#22674,#674);
#629=SHAPE_REPRESENTATION_RELATIONSHIP('SRR','None',#22675,#675);
#630=SHAPE_REPRESENTATION_RELATIONSHIP('SRR','None',#22676,#676);
#631=SHAPE_REPRESENTATION_RELATIONSHIP('SRR','None',#22678,#677);
#632=SHAPE_REPRESENTATION_RELATIONSHIP('SRR','None',#22679,#678);
#633=SHAPE_REPRESENTATION_RELATIONSHIP('SRR','None',#22680,#679);
#634=SHAPE_REPRESENTATION_RELATIONSHIP('SRR','None',#22681,#680);
#635=SHAPE_REPRESENTATION_RELATIONSHIP('SRR','None',#22682,#681);
#636=SHAPE_REPRESENTATION_RELATIONSHIP('SRR','None',#22683,#682);
#637=SHAPE_REPRESENTATION_RELATIONSHIP('SRR','None',#22685,#683);
#638=SHAPE_REPRESENTATION_RELATIONSHIP('SRR','None',#22686,#684);
#639=SHAPE_REPRESENTATION_RELATIONSHIP('SRR','None',#22687,#685);
#640=ADVANCED_BREP_SHAPE_REPRESENTATION('',(#732),#22346);
#641=ADVANCED_BREP_SHAPE_REPRESENTATION('',(#733),#22347);
#642=ADVANCED_BREP_SHAPE_REPRESENTATION('',(#734),#22348);
#643=ADVANCED_BREP_SHAPE_REPRESENTATION('',(#735),#22349);
#644=ADVANCED_BREP_SHAPE_REPRESENTATION('',(#736),#22350);
#645=ADVANCED_BREP_SHAPE_REPRESENTATION('',(#737),#22351);
#646=ADVANCED_BREP_SHAPE_REPRESENTATION('',(#738),#22352);
#647=ADVANCED_BREP_SHAPE_REPRESENTATION('',(#739),#22353);
#648=ADVANCED_BREP_SHAPE_REPRESENTATION('',(#740),#22354);
#649=ADVANCED_BREP_SHAPE_REPRESENTATION('',(#741),#22355);
#650=ADVANCED_BREP_SHAPE_REPRESENTATION('',(#742),#22356);
#651=ADVANCED_BREP_SHAPE_REPRESENTATION('',(#743),#22357);
#652=ADVANCED_BREP_SHAPE_REPRESENTATION('',(#744),#22358);
#653=ADVANCED_BREP_SHAPE_REPRESENTATION('',(#745),#22359);
#654=ADVANCED_BREP_SHAPE_REPRESENTATION('',(#746),#22360);
#655=ADVANCED_BREP_SHAPE_REPRESENTATION('',(#747),#22361);
#656=ADVANCED_BREP_SHAPE_REPRESENTATION('',(#748),#22362);
#657=ADVANCED_BREP_SHAPE_REPRESENTATION('',(#749),#22363);
#658=ADVANCED_BREP_SHAPE_REPRESENTATION('',(#750),#22364);
#659=ADVANCED_BREP_SHAPE_REPRESENTATION('',(#751),#22365);
#660=ADVANCED_BREP_SHAPE_REPRESENTATION('',(#752),#22366);
#661=ADVANCED_BREP_SHAPE_REPRESENTATION('',(#753),#22367);
#662=ADVANCED_BREP_SHAPE_REPRESENTATION('',(#754),#22368);
#663=ADVANCED_BREP_SHAPE_REPRESENTATION('',(#755),#22369);
#664=ADVANCED_BREP_SHAPE_REPRESENTATION('',(#756),#22370);
#665=ADVANCED_BREP_SHAPE_REPRESENTATION('',(#757),#22371);
#666=ADVANCED_BREP_SHAPE_REPRESENTATION('',(#758),#22372);
#667=ADVANCED_BREP_SHAPE_REPRESENTATION('',(#759),#22373);
#668=ADVANCED_BREP_SHAPE_REPRESENTATION('',(#760),#22374);
#669=ADVANCED_BREP_SHAPE_REPRESENTATION('',(#761),#22375);
#670=ADVANCED_BREP_SHAPE_REPRESENTATION('',(#762),#22376);
#671=ADVANCED_BREP_SHAPE_REPRESENTATION('',(#763),#22377);
#672=ADVANCED_BREP_SHAPE_REPRESENTATION('',(#764),#22378);
#673=ADVANCED_BREP_SHAPE_REPRESENTATION('',(#765),#22379);
#674=ADVANCED_BREP_SHAPE_REPRESENTATION('',(#766),#22380);
#675=ADVANCED_BREP_SHAPE_REPRESENTATION('',(#570),#22381);
#676=ADVANCED_BREP_SHAPE_REPRESENTATION('',(#571),#22382);
#677=ADVANCED_BREP_SHAPE_REPRESENTATION('',(#767),#22384);
#678=ADVANCED_BREP_SHAPE_REPRESENTATION('',(#768),#22385);
#679=ADVANCED_BREP_SHAPE_REPRESENTATION('',(#769),#22386);
#680=ADVANCED_BREP_SHAPE_REPRESENTATION('',(#770),#22387);
#681=ADVANCED_BREP_SHAPE_REPRESENTATION('',(#771),#22388);
#682=ADVANCED_BREP_SHAPE_REPRESENTATION('',(#772),#22389);
#683=ADVANCED_BREP_SHAPE_REPRESENTATION('',(#773),#22391);
#684=ADVANCED_BREP_SHAPE_REPRESENTATION('',(#774),#22392);
#685=ADVANCED_BREP_SHAPE_REPRESENTATION('',(#572),#22393);
#686=STYLED_ITEM('',(#22940),#732);
#687=STYLED_ITEM('',(#22947),#733);
#688=STYLED_ITEM('',(#22947),#734);
#689=STYLED_ITEM('',(#22947),#735);
#690=STYLED_ITEM('',(#22940),#736);
#691=STYLED_ITEM('',(#22940),#737);
#692=STYLED_ITEM('',(#22940),#738);
#693=STYLED_ITEM('',(#22940),#739);
#694=STYLED_ITEM('',(#22961),#740);
#695=STYLED_ITEM('',(#22961),#741);
#696=STYLED_ITEM('',(#22940),#742);
#697=STYLED_ITEM('',(#22940),#743);
#698=STYLED_ITEM('',(#22961),#744);
#699=STYLED_ITEM('',(#22961),#745);
#700=STYLED_ITEM('',(#22940),#746);
#701=STYLED_ITEM('',(#22940),#747);
#702=STYLED_ITEM('',(#22961),#748);
#703=STYLED_ITEM('',(#22961),#749);
#704=STYLED_ITEM('',(#22940),#750);
#705=STYLED_ITEM('',(#22940),#751);
#706=STYLED_ITEM('',(#22961),#752);
#707=STYLED_ITEM('',(#22961),#753);
#708=STYLED_ITEM('',(#22954),#754);
#709=STYLED_ITEM('',(#22940),#755);
#710=STYLED_ITEM('',(#22947),#756);
#711=STYLED_ITEM('',(#22947),#757);
#712=STYLED_ITEM('',(#22975),#758);
#713=STYLED_ITEM('',(#22975),#759);
#714=STYLED_ITEM('',(#22975),#760);
#715=STYLED_ITEM('',(#22947),#761);
#716=STYLED_ITEM('',(#22975),#762);
#717=STYLED_ITEM('',(#22975),#763);
#718=STYLED_ITEM('',(#22975),#764);
#719=STYLED_ITEM('',(#22961),#765);
#720=STYLED_ITEM('',(#22961),#766);
#721=STYLED_ITEM('',(#22968),#570);
#722=STYLED_ITEM('',(#22968),#571);
#723=STYLED_ITEM('',(#22975),#767);
#724=STYLED_ITEM('',(#22961),#768);
#725=STYLED_ITEM('',(#22961),#769);
#726=STYLED_ITEM('',(#22961),#770);
#727=STYLED_ITEM('',(#22961),#771);
#728=STYLED_ITEM('',(#22947),#772);
#729=STYLED_ITEM('',(#22975),#773);
#730=STYLED_ITEM('',(#22954),#774);
#731=STYLED_ITEM('',(#22968),#572);
#732=MANIFOLD_SOLID_BREP('Body1',#9204);
#733=MANIFOLD_SOLID_BREP('Body1',#9205);
#734=MANIFOLD_SOLID_BREP('Body1',#9206);
#735=MANIFOLD_SOLID_BREP('Body1',#9207);
#736=MANIFOLD_SOLID_BREP('Body1',#9208);
#737=MANIFOLD_SOLID_BREP('Body1',#9209);
#738=MANIFOLD_SOLID_BREP('Body1',#9210);
#739=MANIFOLD_SOLID_BREP('Body1',#9211);
#740=MANIFOLD_SOLID_BREP('Body1',#9212);
#741=MANIFOLD_SOLID_BREP('Body1',#9213);
#742=MANIFOLD_SOLID_BREP('Body1',#9214);
#743=MANIFOLD_SOLID_BREP('Body1',#9215);
#744=MANIFOLD_SOLID_BREP('Body1',#9216);
#745=MANIFOLD_SOLID_BREP('Body1',#9217);
#746=MANIFOLD_SOLID_BREP('Body1',#9218);
#747=MANIFOLD_SOLID_BREP('Body1',#9219);
#748=MANIFOLD_SOLID_BREP('Body1',#9220);
#749=MANIFOLD_SOLID_BREP('Body1',#9221);
#750=MANIFOLD_SOLID_BREP('Body1',#9222);
#751=MANIFOLD_SOLID_BREP('Body1',#9223);
#752=MANIFOLD_SOLID_BREP('Body1',#9224);
#753=MANIFOLD_SOLID_BREP('Body1',#9225);
#754=MANIFOLD_SOLID_BREP('Body1',#9226);
#755=MANIFOLD_SOLID_BREP('Body1',#9227);
#756=MANIFOLD_SOLID_BREP('Body1',#9228);
#757=MANIFOLD_SOLID_BREP('Body1',#9229);
#758=MANIFOLD_SOLID_BREP('Body1',#9230);
#759=MANIFOLD_SOLID_BREP('Body1',#9231);
#760=MANIFOLD_SOLID_BREP('Body1',#9232);
#761=MANIFOLD_SOLID_BREP('Body1',#9233);
#762=MANIFOLD_SOLID_BREP('Body1',#9234);
#763=MANIFOLD_SOLID_BREP('Body1',#9235);
#764=MANIFOLD_SOLID_BREP('Body1',#9236);
#765=MANIFOLD_SOLID_BREP('Body1',#9237);
#766=MANIFOLD_SOLID_BREP('Body1',#9238);
#767=MANIFOLD_SOLID_BREP('Body1',#9243);
#768=MANIFOLD_SOLID_BREP('Body1',#9244);
#769=MANIFOLD_SOLID_BREP('Body1',#9245);
#770=MANIFOLD_SOLID_BREP('Body1',#9246);
#771=MANIFOLD_SOLID_BREP('Body1',#9247);
#772=MANIFOLD_SOLID_BREP('Body1',#9248);
#773=MANIFOLD_SOLID_BREP('Body1',#9249);
#774=MANIFOLD_SOLID_BREP('Body1',#9250);
#775=FACE_BOUND('',#1866,.T.);
#776=FACE_BOUND('',#1867,.T.);
#777=FACE_BOUND('',#1868,.T.);
#778=FACE_BOUND('',#1869,.T.);
#779=FACE_BOUND('',#1870,.T.);
#780=FACE_BOUND('',#1871,.T.);
#781=FACE_BOUND('',#1872,.T.);
#782=FACE_BOUND('',#1873,.T.);
#783=FACE_BOUND('',#1874,.T.);
#784=FACE_BOUND('',#1875,.T.);
#785=FACE_BOUND('',#1876,.T.);
#786=FACE_BOUND('',#1877,.T.);
#787=FACE_BOUND('',#1878,.T.);
#788=FACE_BOUND('',#1879,.T.);
#789=FACE_BOUND('',#1880,.T.);
#790=FACE_BOUND('',#1881,.T.);
#791=FACE_BOUND('',#1882,.T.);
#792=FACE_BOUND('',#1883,.T.);
#793=FACE_BOUND('',#1884,.T.);
#794=FACE_BOUND('',#1885,.T.);
#795=FACE_BOUND('',#1886,.T.);
#796=FACE_BOUND('',#1887,.T.);
#797=FACE_BOUND('',#1889,.T.);
#798=FACE_BOUND('',#1890,.T.);
#799=FACE_BOUND('',#1891,.T.);
#800=FACE_BOUND('',#1892,.T.);
#801=FACE_BOUND('',#1893,.T.);
#802=FACE_BOUND('',#1894,.T.);
#803=FACE_BOUND('',#1895,.T.);
#804=FACE_BOUND('',#1896,.T.);
#805=FACE_BOUND('',#1897,.T.);
#806=FACE_BOUND('',#1898,.T.);
#807=FACE_BOUND('',#1899,.T.);
#808=FACE_BOUND('',#1900,.T.);
#809=FACE_BOUND('',#1901,.T.);
#810=FACE_BOUND('',#1902,.T.);
#811=FACE_BOUND('',#1903,.T.);
#812=FACE_BOUND('',#1904,.T.);
#813=FACE_BOUND('',#1905,.T.);
#814=FACE_BOUND('',#1906,.T.);
#815=FACE_BOUND('',#1907,.T.);
#816=FACE_BOUND('',#1908,.T.);
#817=FACE_BOUND('',#1909,.T.);
#818=FACE_BOUND('',#1910,.T.);
#819=FACE_BOUND('',#1946,.T.);
#820=FACE_BOUND('',#1947,.T.);
#821=FACE_BOUND('',#1948,.T.);
#822=FACE_BOUND('',#1949,.T.);
#823=FACE_BOUND('',#1950,.T.);
#824=FACE_BOUND('',#1951,.T.);
#825=FACE_BOUND('',#1952,.T.);
#826=FACE_BOUND('',#1953,.T.);
#827=FACE_BOUND('',#1954,.T.);
#828=FACE_BOUND('',#1955,.T.);
#829=FACE_BOUND('',#1956,.T.);
#830=FACE_BOUND('',#1957,.T.);
#831=FACE_BOUND('',#1958,.T.);
#832=FACE_BOUND('',#1959,.T.);
#833=FACE_BOUND('',#1960,.T.);
#834=FACE_BOUND('',#1961,.T.);
#835=FACE_BOUND('',#1962,.T.);
#836=FACE_BOUND('',#1963,.T.);
#837=FACE_BOUND('',#1965,.T.);
#838=FACE_BOUND('',#1966,.T.);
#839=FACE_BOUND('',#1967,.T.);
#840=FACE_BOUND('',#1968,.T.);
#841=FACE_BOUND('',#1969,.T.);
#842=FACE_BOUND('',#1970,.T.);
#843=FACE_BOUND('',#1971,.T.);
#844=FACE_BOUND('',#1972,.T.);
#845=FACE_BOUND('',#1973,.T.);
#846=FACE_BOUND('',#1974,.T.);
#847=FACE_BOUND('',#1975,.T.);
#848=FACE_BOUND('',#1976,.T.);
#849=FACE_BOUND('',#1977,.T.);
#850=FACE_BOUND('',#1978,.T.);
#851=FACE_BOUND('',#1979,.T.);
#852=FACE_BOUND('',#1980,.T.);
#853=FACE_BOUND('',#1981,.T.);
#854=FACE_BOUND('',#1982,.T.);
#855=FACE_BOUND('',#1996,.T.);
#856=FACE_BOUND('',#1997,.T.);
#857=FACE_BOUND('',#1999,.T.);
#858=FACE_BOUND('',#2000,.T.);
#859=FACE_BOUND('',#2014,.T.);
#860=FACE_BOUND('',#2015,.T.);
#861=FACE_BOUND('',#2017,.T.);
#862=FACE_BOUND('',#2018,.T.);
#863=FACE_BOUND('',#2026,.T.);
#864=FACE_BOUND('',#2027,.T.);
#865=FACE_BOUND('',#2030,.T.);
#866=FACE_BOUND('',#2031,.T.);
#867=FACE_BOUND('',#2035,.T.);
#868=FACE_BOUND('',#2036,.T.);
#869=FACE_BOUND('',#2045,.T.);
#870=FACE_BOUND('',#2046,.T.);
#871=FACE_BOUND('',#2050,.T.);
#872=FACE_BOUND('',#2051,.T.);
#873=FACE_BOUND('',#2054,.T.);
#874=FACE_BOUND('',#2055,.T.);
#875=FACE_BOUND('',#2060,.T.);
#876=FACE_BOUND('',#2062,.T.);
#877=FACE_BOUND('',#2073,.T.);
#878=FACE_BOUND('',#2074,.T.);
#879=FACE_BOUND('',#2077,.T.);
#880=FACE_BOUND('',#2078,.T.);
#881=FACE_BOUND('',#2082,.T.);
#882=FACE_BOUND('',#2083,.T.);
#883=FACE_BOUND('',#2092,.T.);
#884=FACE_BOUND('',#2093,.T.);
#885=FACE_BOUND('',#2097,.T.);
#886=FACE_BOUND('',#2098,.T.);
#887=FACE_BOUND('',#2101,.T.);
#888=FACE_BOUND('',#2102,.T.);
#889=FACE_BOUND('',#2107,.T.);
#890=FACE_BOUND('',#2109,.T.);
#891=FACE_BOUND('',#2120,.T.);
#892=FACE_BOUND('',#2121,.T.);
#893=FACE_BOUND('',#2124,.T.);
#894=FACE_BOUND('',#2125,.T.);
#895=FACE_BOUND('',#2129,.T.);
#896=FACE_BOUND('',#2130,.T.);
#897=FACE_BOUND('',#2139,.T.);
#898=FACE_BOUND('',#2140,.T.);
#899=FACE_BOUND('',#2144,.T.);
#900=FACE_BOUND('',#2145,.T.);
#901=FACE_BOUND('',#2148,.T.);
#902=FACE_BOUND('',#2149,.T.);
#903=FACE_BOUND('',#2154,.T.);
#904=FACE_BOUND('',#2156,.T.);
#905=FACE_BOUND('',#2167,.T.);
#906=FACE_BOUND('',#2168,.T.);
#907=FACE_BOUND('',#2171,.T.);
#908=FACE_BOUND('',#2172,.T.);
#909=FACE_BOUND('',#2176,.T.);
#910=FACE_BOUND('',#2177,.T.);
#911=FACE_BOUND('',#2186,.T.);
#912=FACE_BOUND('',#2187,.T.);
#913=FACE_BOUND('',#2191,.T.);
#914=FACE_BOUND('',#2192,.T.);
#915=FACE_BOUND('',#2195,.T.);
#916=FACE_BOUND('',#2196,.T.);
#917=FACE_BOUND('',#2201,.T.);
#918=FACE_BOUND('',#2203,.T.);
#919=FACE_BOUND('',#2219,.T.);
#920=FACE_BOUND('',#2225,.T.);
#921=FACE_BOUND('',#2227,.T.);
#922=FACE_BOUND('',#2228,.T.);
#923=FACE_BOUND('',#2229,.T.);
#924=FACE_BOUND('',#2230,.T.);
#925=FACE_BOUND('',#2244,.T.);
#926=FACE_BOUND('',#2245,.T.);
#927=FACE_BOUND('',#2246,.T.);
#928=FACE_BOUND('',#2247,.T.);
#929=FACE_BOUND('',#2248,.T.);
#930=FACE_BOUND('',#2249,.T.);
#931=FACE_BOUND('',#2250,.T.);
#932=FACE_BOUND('',#2251,.T.);
#933=FACE_BOUND('',#2253,.T.);
#934=FACE_BOUND('',#2254,.T.);
#935=FACE_BOUND('',#2255,.T.);
#936=FACE_BOUND('',#2256,.T.);
#937=FACE_BOUND('',#2257,.T.);
#938=FACE_BOUND('',#2258,.T.);
#939=FACE_BOUND('',#2259,.T.);
#940=FACE_BOUND('',#2260,.T.);
#941=FACE_BOUND('',#2264,.T.);
#942=FACE_BOUND('',#2266,.T.);
#943=FACE_BOUND('',#2272,.T.);
#944=FACE_BOUND('',#2280,.T.);
#945=FACE_BOUND('',#2290,.T.);
#946=FACE_BOUND('',#2298,.T.);
#947=FACE_BOUND('',#2313,.T.);
#948=FACE_BOUND('',#2315,.T.);
#949=FACE_BOUND('',#2317,.T.);
#950=FACE_BOUND('',#2324,.T.);
#951=FACE_BOUND('',#2327,.T.);
#952=FACE_BOUND('',#2328,.T.);
#953=FACE_BOUND('',#2331,.T.);
#954=FACE_BOUND('',#2334,.T.);
#955=FACE_BOUND('',#2337,.T.);
#956=FACE_BOUND('',#2340,.T.);
#957=FACE_BOUND('',#2355,.T.);
#958=FACE_BOUND('',#2363,.T.);
#959=FACE_BOUND('',#2405,.T.);
#960=FACE_BOUND('',#2406,.T.);
#961=FACE_BOUND('',#2407,.T.);
#962=FACE_BOUND('',#2408,.T.);
#963=FACE_BOUND('',#2409,.T.);
#964=FACE_BOUND('',#2410,.T.);
#965=FACE_BOUND('',#2411,.T.);
#966=FACE_BOUND('',#2412,.T.);
#967=FACE_BOUND('',#2413,.T.);
#968=FACE_BOUND('',#2414,.T.);
#969=FACE_BOUND('',#2415,.T.);
#970=FACE_BOUND('',#2416,.T.);
#971=FACE_BOUND('',#2417,.T.);
#972=FACE_BOUND('',#2418,.T.);
#973=FACE_BOUND('',#2419,.T.);
#974=FACE_BOUND('',#2420,.T.);
#975=FACE_BOUND('',#2421,.T.);
#976=FACE_BOUND('',#2422,.T.);
#977=FACE_BOUND('',#2423,.T.);
#978=FACE_BOUND('',#2424,.T.);
#979=FACE_BOUND('',#2425,.T.);
#980=FACE_BOUND('',#2426,.T.);
#981=FACE_BOUND('',#2427,.T.);
#982=FACE_BOUND('',#2428,.T.);
#983=FACE_BOUND('',#2430,.T.);
#984=FACE_BOUND('',#2431,.T.);
#985=FACE_BOUND('',#2432,.T.);
#986=FACE_BOUND('',#2433,.T.);
#987=FACE_BOUND('',#2434,.T.);
#988=FACE_BOUND('',#2435,.T.);
#989=FACE_BOUND('',#2436,.T.);
#990=FACE_BOUND('',#2437,.T.);
#991=FACE_BOUND('',#2438,.T.);
#992=FACE_BOUND('',#2439,.T.);
#993=FACE_BOUND('',#2440,.T.);
#994=FACE_BOUND('',#2441,.T.);
#995=FACE_BOUND('',#2442,.T.);
#996=FACE_BOUND('',#2443,.T.);
#997=FACE_BOUND('',#2444,.T.);
#998=FACE_BOUND('',#2445,.T.);
#999=FACE_BOUND('',#2446,.T.);
#1000=FACE_BOUND('',#2447,.T.);
#1001=FACE_BOUND('',#2448,.T.);
#1002=FACE_BOUND('',#2449,.T.);
#1003=FACE_BOUND('',#2450,.T.);
#1004=FACE_BOUND('',#2451,.T.);
#1005=FACE_BOUND('',#2452,.T.);
#1006=FACE_BOUND('',#2453,.T.);
#1007=FACE_BOUND('',#2465,.T.);
#1008=FACE_BOUND('',#2467,.T.);
#1009=FACE_BOUND('',#2471,.T.);
#1010=FACE_BOUND('',#2472,.T.);
#1011=FACE_BOUND('',#2473,.T.);
#1012=FACE_BOUND('',#2474,.T.);
#1013=FACE_BOUND('',#2475,.T.);
#1014=FACE_BOUND('',#2477,.T.);
#1015=FACE_BOUND('',#2489,.T.);
#1016=FACE_BOUND('',#2491,.T.);
#1017=FACE_BOUND('',#2495,.T.);
#1018=FACE_BOUND('',#2496,.T.);
#1019=FACE_BOUND('',#2497,.T.);
#1020=FACE_BOUND('',#2498,.T.);
#1021=FACE_BOUND('',#2499,.T.);
#1022=FACE_BOUND('',#2501,.T.);
#1023=FACE_BOUND('',#2513,.T.);
#1024=FACE_BOUND('',#2515,.T.);
#1025=FACE_BOUND('',#2519,.T.);
#1026=FACE_BOUND('',#2520,.T.);
#1027=FACE_BOUND('',#2521,.T.);
#1028=FACE_BOUND('',#2522,.T.);
#1029=FACE_BOUND('',#2523,.T.);
#1030=FACE_BOUND('',#2525,.T.);
#1031=FACE_BOUND('',#2537,.T.);
#1032=FACE_BOUND('',#2539,.T.);
#1033=FACE_BOUND('',#2543,.T.);
#1034=FACE_BOUND('',#2544,.T.);
#1035=FACE_BOUND('',#2545,.T.);
#1036=FACE_BOUND('',#2546,.T.);
#1037=FACE_BOUND('',#2547,.T.);
#1038=FACE_BOUND('',#2549,.T.);
#1039=FACE_BOUND('',#2555,.T.);
#1040=FACE_BOUND('',#2556,.T.);
#1041=FACE_BOUND('',#2557,.T.);
#1042=FACE_BOUND('',#2558,.T.);
#1043=FACE_BOUND('',#2559,.T.);
#1044=FACE_BOUND('',#2563,.T.);
#1045=FACE_BOUND('',#2564,.T.);
#1046=FACE_BOUND('',#2565,.T.);
#1047=FACE_BOUND('',#2566,.T.);
#1048=FACE_BOUND('',#2574,.T.);
#1049=FACE_BOUND('',#2577,.T.);
#1050=FACE_BOUND('',#2580,.T.);
#1051=FACE_BOUND('',#2583,.T.);
#1052=FACE_BOUND('',#2586,.T.);
#1053=FACE_BOUND('',#2589,.T.);
#1054=FACE_BOUND('',#2591,.T.);
#1055=FACE_BOUND('',#2597,.T.);
#1056=FACE_BOUND('',#2599,.T.);
#1057=FACE_BOUND('',#2601,.T.);
#1058=FACE_BOUND('',#2603,.T.);
#1059=FACE_BOUND('',#2609,.T.);
#1060=PLANE('',#9829);
#1061=PLANE('',#9830);
#1062=PLANE('',#9831);
#1063=PLANE('',#9832);
#1064=PLANE('',#9833);
#1065=PLANE('',#9834);
#1066=PLANE('',#9836);
#1067=PLANE('',#9837);
#1068=PLANE('',#9838);
#1069=PLANE('',#9839);
#1070=PLANE('',#9840);
#1071=PLANE('',#9841);
#1072=PLANE('',#9843);
#1073=PLANE('',#9844);
#1074=PLANE('',#9845);
#1075=PLANE('',#9846);
#1076=PLANE('',#9847);
#1077=PLANE('',#9848);
#1078=PLANE('',#9904);
#1079=PLANE('',#9905);
#1080=PLANE('',#9906);
#1081=PLANE('',#9907);
#1082=PLANE('',#9908);
#1083=PLANE('',#9909);
#1084=PLANE('',#9914);
#1085=PLANE('',#9918);
#1086=PLANE('',#9922);
#1087=PLANE('',#9926);
#1088=PLANE('',#9927);
#1089=PLANE('',#9928);
#1090=PLANE('',#9929);
#1091=PLANE('',#9930);
#1092=PLANE('',#9931);
#1093=PLANE('',#9932);
#1094=PLANE('',#9937);
#1095=PLANE('',#9941);
#1096=PLANE('',#9945);
#1097=PLANE('',#9949);
#1098=PLANE('',#9950);
#1099=PLANE('',#9951);
#1100=PLANE('',#9952);
#1101=PLANE('',#9953);
#1102=PLANE('',#9954);
#1103=PLANE('',#9955);
#1104=PLANE('',#9960);
#1105=PLANE('',#9964);
#1106=PLANE('',#9971);
#1107=PLANE('',#9972);
#1108=PLANE('',#9973);
#1109=PLANE('',#9974);
#1110=PLANE('',#9975);
#1111=PLANE('',#9976);
#1112=PLANE('',#9989);
#1113=PLANE('',#9995);
#1114=PLANE('',#9996);
#1115=PLANE('',#9997);
#1116=PLANE('',#9998);
#1117=PLANE('',#9999);
#1118=PLANE('',#10000);
#1119=PLANE('',#10001);
#1120=PLANE('',#10002);
#1121=PLANE('',#10003);
#1122=PLANE('',#10011);
#1123=PLANE('',#10012);
#1124=PLANE('',#10016);
#1125=PLANE('',#10017);
#1126=PLANE('',#10022);
#1127=PLANE('',#10026);
#1128=PLANE('',#10033);
#1129=PLANE('',#10034);
#1130=PLANE('',#10035);
#1131=PLANE('',#10036);
#1132=PLANE('',#10037);
#1133=PLANE('',#10038);
#1134=PLANE('',#10051);
#1135=PLANE('',#10057);
#1136=PLANE('',#10058);
#1137=PLANE('',#10059);
#1138=PLANE('',#10060);
#1139=PLANE('',#10061);
#1140=PLANE('',#10062);
#1141=PLANE('',#10063);
#1142=PLANE('',#10064);
#1143=PLANE('',#10065);
#1144=PLANE('',#10073);
#1145=PLANE('',#10074);
#1146=PLANE('',#10078);
#1147=PLANE('',#10079);
#1148=PLANE('',#10084);
#1149=PLANE('',#10088);
#1150=PLANE('',#10095);
#1151=PLANE('',#10096);
#1152=PLANE('',#10097);
#1153=PLANE('',#10098);
#1154=PLANE('',#10099);
#1155=PLANE('',#10100);
#1156=PLANE('',#10113);
#1157=PLANE('',#10119);
#1158=PLANE('',#10120);
#1159=PLANE('',#10121);
#1160=PLANE('',#10122);
#1161=PLANE('',#10123);
#1162=PLANE('',#10124);
#1163=PLANE('',#10125);
#1164=PLANE('',#10126);
#1165=PLANE('',#10127);
#1166=PLANE('',#10135);
#1167=PLANE('',#10136);
#1168=PLANE('',#10140);
#1169=PLANE('',#10141);
#1170=PLANE('',#10146);
#1171=PLANE('',#10150);
#1172=PLANE('',#10157);
#1173=PLANE('',#10158);
#1174=PLANE('',#10159);
#1175=PLANE('',#10160);
#1176=PLANE('',#10161);
#1177=PLANE('',#10162);
#1178=PLANE('',#10175);
#1179=PLANE('',#10181);
#1180=PLANE('',#10182);
#1181=PLANE('',#10183);
#1182=PLANE('',#10184);
#1183=PLANE('',#10185);
#1184=PLANE('',#10186);
#1185=PLANE('',#10187);
#1186=PLANE('',#10188);
#1187=PLANE('',#10189);
#1188=PLANE('',#10197);
#1189=PLANE('',#10198);
#1190=PLANE('',#10202);
#1191=PLANE('',#10203);
#1192=PLANE('',#10208);
#1193=PLANE('',#10212);
#1194=PLANE('',#10216);
#1195=PLANE('',#10220);
#1196=PLANE('',#10224);
#1197=PLANE('',#10228);
#1198=PLANE('',#10229);
#1199=PLANE('',#10230);
#1200=PLANE('',#10231);
#1201=PLANE('',#10232);
#1202=PLANE('',#10233);
#1203=PLANE('',#10234);
#1204=PLANE('',#10260);
#1205=PLANE('',#10261);
#1206=PLANE('',#10262);
#1207=PLANE('',#10263);
#1208=PLANE('',#10264);
#1209=PLANE('',#10265);
#1210=PLANE('',#10273);
#1211=PLANE('',#10274);
#1212=PLANE('',#10279);
#1213=PLANE('',#10283);
#1214=PLANE('',#10284);
#1215=PLANE('',#10289);
#1216=PLANE('',#10290);
#1217=PLANE('',#10295);
#1218=PLANE('',#10299);
#1219=PLANE('',#10300);
#1220=PLANE('',#10305);
#1221=PLANE('',#10306);
#1222=PLANE('',#10311);
#1223=PLANE('',#10315);
#1224=PLANE('',#10316);
#1225=PLANE('',#10321);
#1226=PLANE('',#10322);
#1227=PLANE('',#10327);
#1228=PLANE('',#10331);
#1229=PLANE('',#10332);
#1230=PLANE('',#10337);
#1231=PLANE('',#10338);
#1232=PLANE('',#10345);
#1233=PLANE('',#10348);
#1234=PLANE('',#10350);
#1235=PLANE('',#10357);
#1236=PLANE('',#10358);
#1237=PLANE('',#10360);
#1238=PLANE('',#10362);
#1239=PLANE('',#10376);
#1240=PLANE('',#10377);
#1241=PLANE('',#10378);
#1242=PLANE('',#10379);
#1243=PLANE('',#10380);
#1244=PLANE('',#10381);
#1245=PLANE('',#10382);
#1246=PLANE('',#10383);
#1247=PLANE('',#10384);
#1248=PLANE('',#10385);
#1249=PLANE('',#10386);
#1250=PLANE('',#10388);
#1251=PLANE('',#10389);
#1252=PLANE('',#10390);
#1253=PLANE('',#10391);
#1254=PLANE('',#10392);
#1255=PLANE('',#10393);
#1256=PLANE('',#10394);
#1257=PLANE('',#10395);
#1258=PLANE('',#10396);
#1259=PLANE('',#10398);
#1260=PLANE('',#10406);
#1261=PLANE('',#10412);
#1262=PLANE('',#10420);
#1263=PLANE('',#10428);
#1264=PLANE('',#10429);
#1265=PLANE('',#10430);
#1266=PLANE('',#10431);
#1267=PLANE('',#10432);
#1268=PLANE('',#10433);
#1269=PLANE('',#10434);
#1270=PLANE('',#10435);
#1271=PLANE('',#10436);
#1272=PLANE('',#10511);
#1273=PLANE('',#10512);
#1274=PLANE('',#10513);
#1275=PLANE('',#10514);
#1276=PLANE('',#10515);
#1277=PLANE('',#10516);
#1278=PLANE('',#10518);
#1279=PLANE('',#10525);
#1280=PLANE('',#10532);
#1281=PLANE('',#10539);
#1282=PLANE('',#10556);
#1283=PLANE('',#10558);
#1284=PLANE('',#10564);
#1285=PLANE('',#10565);
#1286=PLANE('',#10567);
#1287=PLANE('',#10574);
#1288=PLANE('',#10581);
#1289=PLANE('',#10588);
#1290=PLANE('',#10605);
#1291=PLANE('',#10607);
#1292=PLANE('',#10613);
#1293=PLANE('',#10614);
#1294=PLANE('',#10616);
#1295=PLANE('',#10623);
#1296=PLANE('',#10630);
#1297=PLANE('',#10637);
#1298=PLANE('',#10654);
#1299=PLANE('',#10656);
#1300=PLANE('',#10662);
#1301=PLANE('',#10663);
#1302=PLANE('',#10665);
#1303=PLANE('',#10672);
#1304=PLANE('',#10679);
#1305=PLANE('',#10686);
#1306=PLANE('',#10703);
#1307=PLANE('',#10705);
#1308=PLANE('',#10711);
#1309=PLANE('',#10712);
#1310=PLANE('',#10726);
#1311=PLANE('',#10733);
#1312=PLANE('',#10734);
#1313=PLANE('',#10737);
#1314=PLANE('',#10739);
#1315=PLANE('',#10740);
#1316=PLANE('',#10742);
#1317=PLANE('',#10743);
#1318=PLANE('',#10744);
#1319=PLANE('',#10749);
#1320=PLANE('',#10753);
#1321=PLANE('',#10757);
#1322=PLANE('',#10761);
#1323=PLANE('',#10765);
#1324=PLANE('',#10769);
#1325=PLANE('',#10772);
#1326=PLANE('',#10773);
#1327=PLANE('',#10776);
#1328=PLANE('',#10777);
#1329=PLANE('',#10782);
#1330=PLANE('',#10788);
#1331=PLANE('',#10796);
#1332=PLANE('',#10804);
#1333=PLANE('',#10805);
#1334=PLANE('',#10806);
#1335=PLANE('',#10807);
#1336=PLANE('',#10808);
#1337=PLANE('',#10809);
#1338=PLANE('',#10810);
#1339=PLANE('',#10811);
#1340=PLANE('',#10812);
#1341=FACE_OUTER_BOUND('',#1839,.T.);
#1342=FACE_OUTER_BOUND('',#1840,.T.);
#1343=FACE_OUTER_BOUND('',#1841,.T.);
#1344=FACE_OUTER_BOUND('',#1842,.T.);
#1345=FACE_OUTER_BOUND('',#1843,.T.);
#1346=FACE_OUTER_BOUND('',#1844,.T.);
#1347=FACE_OUTER_BOUND('',#1845,.T.);
#1348=FACE_OUTER_BOUND('',#1846,.T.);
#1349=FACE_OUTER_BOUND('',#1847,.T.);
#1350=FACE_OUTER_BOUND('',#1848,.T.);
#1351=FACE_OUTER_BOUND('',#1849,.T.);
#1352=FACE_OUTER_BOUND('',#1850,.T.);
#1353=FACE_OUTER_BOUND('',#1851,.T.);
#1354=FACE_OUTER_BOUND('',#1852,.T.);
#1355=FACE_OUTER_BOUND('',#1853,.T.);
#1356=FACE_OUTER_BOUND('',#1854,.T.);
#1357=FACE_OUTER_BOUND('',#1855,.T.);
#1358=FACE_OUTER_BOUND('',#1856,.T.);
#1359=FACE_OUTER_BOUND('',#1857,.T.);
#1360=FACE_OUTER_BOUND('',#1858,.T.);
#1361=FACE_OUTER_BOUND('',#1859,.T.);
#1362=FACE_OUTER_BOUND('',#1860,.T.);
#1363=FACE_OUTER_BOUND('',#1861,.T.);
#1364=FACE_OUTER_BOUND('',#1862,.T.);
#1365=FACE_OUTER_BOUND('',#1863,.T.);
#1366=FACE_OUTER_BOUND('',#1864,.T.);
#1367=FACE_OUTER_BOUND('',#1865,.T.);
#1368=FACE_OUTER_BOUND('',#1888,.T.);
#1369=FACE_OUTER_BOUND('',#1911,.T.);
#1370=FACE_OUTER_BOUND('',#1912,.T.);
#1371=FACE_OUTER_BOUND('',#1913,.T.);
#1372=FACE_OUTER_BOUND('',#1914,.T.);
#1373=FACE_OUTER_BOUND('',#1915,.T.);
#1374=FACE_OUTER_BOUND('',#1916,.T.);
#1375=FACE_OUTER_BOUND('',#1917,.T.);
#1376=FACE_OUTER_BOUND('',#1918,.T.);
#1377=FACE_OUTER_BOUND('',#1919,.T.);
#1378=FACE_OUTER_BOUND('',#1920,.T.);
#1379=FACE_OUTER_BOUND('',#1921,.T.);
#1380=FACE_OUTER_BOUND('',#1922,.T.);
#1381=FACE_OUTER_BOUND('',#1923,.T.);
#1382=FACE_OUTER_BOUND('',#1924,.T.);
#1383=FACE_OUTER_BOUND('',#1925,.T.);
#1384=FACE_OUTER_BOUND('',#1926,.T.);
#1385=FACE_OUTER_BOUND('',#1927,.T.);
#1386=FACE_OUTER_BOUND('',#1928,.T.);
#1387=FACE_OUTER_BOUND('',#1929,.T.);
#1388=FACE_OUTER_BOUND('',#1930,.T.);
#1389=FACE_OUTER_BOUND('',#1931,.T.);
#1390=FACE_OUTER_BOUND('',#1932,.T.);
#1391=FACE_OUTER_BOUND('',#1933,.T.);
#1392=FACE_OUTER_BOUND('',#1934,.T.);
#1393=FACE_OUTER_BOUND('',#1935,.T.);
#1394=FACE_OUTER_BOUND('',#1936,.T.);
#1395=FACE_OUTER_BOUND('',#1937,.T.);
#1396=FACE_OUTER_BOUND('',#1938,.T.);
#1397=FACE_OUTER_BOUND('',#1939,.T.);
#1398=FACE_OUTER_BOUND('',#1940,.T.);
#1399=FACE_OUTER_BOUND('',#1941,.T.);
#1400=FACE_OUTER_BOUND('',#1942,.T.);
#1401=FACE_OUTER_BOUND('',#1943,.T.);
#1402=FACE_OUTER_BOUND('',#1944,.T.);
#1403=FACE_OUTER_BOUND('',#1945,.T.);
#1404=FACE_OUTER_BOUND('',#1964,.T.);
#1405=FACE_OUTER_BOUND('',#1983,.T.);
#1406=FACE_OUTER_BOUND('',#1984,.T.);
#1407=FACE_OUTER_BOUND('',#1985,.T.);
#1408=FACE_OUTER_BOUND('',#1986,.T.);
#1409=FACE_OUTER_BOUND('',#1987,.T.);
#1410=FACE_OUTER_BOUND('',#1988,.T.);
#1411=FACE_OUTER_BOUND('',#1989,.T.);
#1412=FACE_OUTER_BOUND('',#1990,.T.);
#1413=FACE_OUTER_BOUND('',#1991,.T.);
#1414=FACE_OUTER_BOUND('',#1992,.T.);
#1415=FACE_OUTER_BOUND('',#1993,.T.);
#1416=FACE_OUTER_BOUND('',#1994,.T.);
#1417=FACE_OUTER_BOUND('',#1995,.T.);
#1418=FACE_OUTER_BOUND('',#1998,.T.);
#1419=FACE_OUTER_BOUND('',#2001,.T.);
#1420=FACE_OUTER_BOUND('',#2002,.T.);
#1421=FACE_OUTER_BOUND('',#2003,.T.);
#1422=FACE_OUTER_BOUND('',#2004,.T.);
#1423=FACE_OUTER_BOUND('',#2005,.T.);
#1424=FACE_OUTER_BOUND('',#2006,.T.);
#1425=FACE_OUTER_BOUND('',#2007,.T.);
#1426=FACE_OUTER_BOUND('',#2008,.T.);
#1427=FACE_OUTER_BOUND('',#2009,.T.);
#1428=FACE_OUTER_BOUND('',#2010,.T.);
#1429=FACE_OUTER_BOUND('',#2011,.T.);
#1430=FACE_OUTER_BOUND('',#2012,.T.);
#1431=FACE_OUTER_BOUND('',#2013,.T.);
#1432=FACE_OUTER_BOUND('',#2016,.T.);
#1433=FACE_OUTER_BOUND('',#2019,.T.);
#1434=FACE_OUTER_BOUND('',#2020,.T.);
#1435=FACE_OUTER_BOUND('',#2021,.T.);
#1436=FACE_OUTER_BOUND('',#2022,.T.);
#1437=FACE_OUTER_BOUND('',#2023,.T.);
#1438=FACE_OUTER_BOUND('',#2024,.T.);
#1439=FACE_OUTER_BOUND('',#2025,.T.);
#1440=FACE_OUTER_BOUND('',#2028,.T.);
#1441=FACE_OUTER_BOUND('',#2029,.T.);
#1442=FACE_OUTER_BOUND('',#2032,.T.);
#1443=FACE_OUTER_BOUND('',#2033,.T.);
#1444=FACE_OUTER_BOUND('',#2034,.T.);
#1445=FACE_OUTER_BOUND('',#2037,.T.);
#1446=FACE_OUTER_BOUND('',#2038,.T.);
#1447=FACE_OUTER_BOUND('',#2039,.T.);
#1448=FACE_OUTER_BOUND('',#2040,.T.);
#1449=FACE_OUTER_BOUND('',#2041,.T.);
#1450=FACE_OUTER_BOUND('',#2042,.T.);
#1451=FACE_OUTER_BOUND('',#2043,.T.);
#1452=FACE_OUTER_BOUND('',#2044,.T.);
#1453=FACE_OUTER_BOUND('',#2047,.T.);
#1454=FACE_OUTER_BOUND('',#2048,.T.);
#1455=FACE_OUTER_BOUND('',#2049,.T.);
#1456=FACE_OUTER_BOUND('',#2052,.T.);
#1457=FACE_OUTER_BOUND('',#2053,.T.);
#1458=FACE_OUTER_BOUND('',#2056,.T.);
#1459=FACE_OUTER_BOUND('',#2057,.T.);
#1460=FACE_OUTER_BOUND('',#2058,.T.);
#1461=FACE_OUTER_BOUND('',#2059,.T.);
#1462=FACE_OUTER_BOUND('',#2061,.T.);
#1463=FACE_OUTER_BOUND('',#2063,.T.);
#1464=FACE_OUTER_BOUND('',#2064,.T.);
#1465=FACE_OUTER_BOUND('',#2065,.T.);
#1466=FACE_OUTER_BOUND('',#2066,.T.);
#1467=FACE_OUTER_BOUND('',#2067,.T.);
#1468=FACE_OUTER_BOUND('',#2068,.T.);
#1469=FACE_OUTER_BOUND('',#2069,.T.);
#1470=FACE_OUTER_BOUND('',#2070,.T.);
#1471=FACE_OUTER_BOUND('',#2071,.T.);
#1472=FACE_OUTER_BOUND('',#2072,.T.);
#1473=FACE_OUTER_BOUND('',#2075,.T.);
#1474=FACE_OUTER_BOUND('',#2076,.T.);
#1475=FACE_OUTER_BOUND('',#2079,.T.);
#1476=FACE_OUTER_BOUND('',#2080,.T.);
#1477=FACE_OUTER_BOUND('',#2081,.T.);
#1478=FACE_OUTER_BOUND('',#2084,.T.);
#1479=FACE_OUTER_BOUND('',#2085,.T.);
#1480=FACE_OUTER_BOUND('',#2086,.T.);
#1481=FACE_OUTER_BOUND('',#2087,.T.);
#1482=FACE_OUTER_BOUND('',#2088,.T.);
#1483=FACE_OUTER_BOUND('',#2089,.T.);
#1484=FACE_OUTER_BOUND('',#2090,.T.);
#1485=FACE_OUTER_BOUND('',#2091,.T.);
#1486=FACE_OUTER_BOUND('',#2094,.T.);
#1487=FACE_OUTER_BOUND('',#2095,.T.);
#1488=FACE_OUTER_BOUND('',#2096,.T.);
#1489=FACE_OUTER_BOUND('',#2099,.T.);
#1490=FACE_OUTER_BOUND('',#2100,.T.);
#1491=FACE_OUTER_BOUND('',#2103,.T.);
#1492=FACE_OUTER_BOUND('',#2104,.T.);
#1493=FACE_OUTER_BOUND('',#2105,.T.);
#1494=FACE_OUTER_BOUND('',#2106,.T.);
#1495=FACE_OUTER_BOUND('',#2108,.T.);
#1496=FACE_OUTER_BOUND('',#2110,.T.);
#1497=FACE_OUTER_BOUND('',#2111,.T.);
#1498=FACE_OUTER_BOUND('',#2112,.T.);
#1499=FACE_OUTER_BOUND('',#2113,.T.);
#1500=FACE_OUTER_BOUND('',#2114,.T.);
#1501=FACE_OUTER_BOUND('',#2115,.T.);
#1502=FACE_OUTER_BOUND('',#2116,.T.);
#1503=FACE_OUTER_BOUND('',#2117,.T.);
#1504=FACE_OUTER_BOUND('',#2118,.T.);
#1505=FACE_OUTER_BOUND('',#2119,.T.);
#1506=FACE_OUTER_BOUND('',#2122,.T.);
#1507=FACE_OUTER_BOUND('',#2123,.T.);
#1508=FACE_OUTER_BOUND('',#2126,.T.);
#1509=FACE_OUTER_BOUND('',#2127,.T.);
#1510=FACE_OUTER_BOUND('',#2128,.T.);
#1511=FACE_OUTER_BOUND('',#2131,.T.);
#1512=FACE_OUTER_BOUND('',#2132,.T.);
#1513=FACE_OUTER_BOUND('',#2133,.T.);
#1514=FACE_OUTER_BOUND('',#2134,.T.);
#1515=FACE_OUTER_BOUND('',#2135,.T.);
#1516=FACE_OUTER_BOUND('',#2136,.T.);
#1517=FACE_OUTER_BOUND('',#2137,.T.);
#1518=FACE_OUTER_BOUND('',#2138,.T.);
#1519=FACE_OUTER_BOUND('',#2141,.T.);
#1520=FACE_OUTER_BOUND('',#2142,.T.);
#1521=FACE_OUTER_BOUND('',#2143,.T.);
#1522=FACE_OUTER_BOUND('',#2146,.T.);
#1523=FACE_OUTER_BOUND('',#2147,.T.);
#1524=FACE_OUTER_BOUND('',#2150,.T.);
#1525=FACE_OUTER_BOUND('',#2151,.T.);
#1526=FACE_OUTER_BOUND('',#2152,.T.);
#1527=FACE_OUTER_BOUND('',#2153,.T.);
#1528=FACE_OUTER_BOUND('',#2155,.T.);
#1529=FACE_OUTER_BOUND('',#2157,.T.);
#1530=FACE_OUTER_BOUND('',#2158,.T.);
#1531=FACE_OUTER_BOUND('',#2159,.T.);
#1532=FACE_OUTER_BOUND('',#2160,.T.);
#1533=FACE_OUTER_BOUND('',#2161,.T.);
#1534=FACE_OUTER_BOUND('',#2162,.T.);
#1535=FACE_OUTER_BOUND('',#2163,.T.);
#1536=FACE_OUTER_BOUND('',#2164,.T.);
#1537=FACE_OUTER_BOUND('',#2165,.T.);
#1538=FACE_OUTER_BOUND('',#2166,.T.);
#1539=FACE_OUTER_BOUND('',#2169,.T.);
#1540=FACE_OUTER_BOUND('',#2170,.T.);
#1541=FACE_OUTER_BOUND('',#2173,.T.);
#1542=FACE_OUTER_BOUND('',#2174,.T.);
#1543=FACE_OUTER_BOUND('',#2175,.T.);
#1544=FACE_OUTER_BOUND('',#2178,.T.);
#1545=FACE_OUTER_BOUND('',#2179,.T.);
#1546=FACE_OUTER_BOUND('',#2180,.T.);
#1547=FACE_OUTER_BOUND('',#2181,.T.);
#1548=FACE_OUTER_BOUND('',#2182,.T.);
#1549=FACE_OUTER_BOUND('',#2183,.T.);
#1550=FACE_OUTER_BOUND('',#2184,.T.);
#1551=FACE_OUTER_BOUND('',#2185,.T.);
#1552=FACE_OUTER_BOUND('',#2188,.T.);
#1553=FACE_OUTER_BOUND('',#2189,.T.);
#1554=FACE_OUTER_BOUND('',#2190,.T.);
#1555=FACE_OUTER_BOUND('',#2193,.T.);
#1556=FACE_OUTER_BOUND('',#2194,.T.);
#1557=FACE_OUTER_BOUND('',#2197,.T.);
#1558=FACE_OUTER_BOUND('',#2198,.T.);
#1559=FACE_OUTER_BOUND('',#2199,.T.);
#1560=FACE_OUTER_BOUND('',#2200,.T.);
#1561=FACE_OUTER_BOUND('',#2202,.T.);
#1562=FACE_OUTER_BOUND('',#2204,.T.);
#1563=FACE_OUTER_BOUND('',#2205,.T.);
#1564=FACE_OUTER_BOUND('',#2206,.T.);
#1565=FACE_OUTER_BOUND('',#2207,.T.);
#1566=FACE_OUTER_BOUND('',#2208,.T.);
#1567=FACE_OUTER_BOUND('',#2209,.T.);
#1568=FACE_OUTER_BOUND('',#2210,.T.);
#1569=FACE_OUTER_BOUND('',#2211,.T.);
#1570=FACE_OUTER_BOUND('',#2212,.T.);
#1571=FACE_OUTER_BOUND('',#2213,.T.);
#1572=FACE_OUTER_BOUND('',#2214,.T.);
#1573=FACE_OUTER_BOUND('',#2215,.T.);
#1574=FACE_OUTER_BOUND('',#2216,.T.);
#1575=FACE_OUTER_BOUND('',#2217,.T.);
#1576=FACE_OUTER_BOUND('',#2218,.T.);
#1577=FACE_OUTER_BOUND('',#2220,.T.);
#1578=FACE_OUTER_BOUND('',#2221,.T.);
#1579=FACE_OUTER_BOUND('',#2222,.T.);
#1580=FACE_OUTER_BOUND('',#2223,.T.);
#1581=FACE_OUTER_BOUND('',#2224,.T.);
#1582=FACE_OUTER_BOUND('',#2226,.T.);
#1583=FACE_OUTER_BOUND('',#2231,.T.);
#1584=FACE_OUTER_BOUND('',#2232,.T.);
#1585=FACE_OUTER_BOUND('',#2233,.T.);
#1586=FACE_OUTER_BOUND('',#2234,.T.);
#1587=FACE_OUTER_BOUND('',#2235,.T.);
#1588=FACE_OUTER_BOUND('',#2236,.T.);
#1589=FACE_OUTER_BOUND('',#2237,.T.);
#1590=FACE_OUTER_BOUND('',#2238,.T.);
#1591=FACE_OUTER_BOUND('',#2239,.T.);
#1592=FACE_OUTER_BOUND('',#2240,.T.);
#1593=FACE_OUTER_BOUND('',#2241,.T.);
#1594=FACE_OUTER_BOUND('',#2242,.T.);
#1595=FACE_OUTER_BOUND('',#2243,.T.);
#1596=FACE_OUTER_BOUND('',#2252,.T.);
#1597=FACE_OUTER_BOUND('',#2261,.T.);
#1598=FACE_OUTER_BOUND('',#2262,.T.);
#1599=FACE_OUTER_BOUND('',#2263,.T.);
#1600=FACE_OUTER_BOUND('',#2265,.T.);
#1601=FACE_OUTER_BOUND('',#2267,.T.);
#1602=FACE_OUTER_BOUND('',#2268,.T.);
#1603=FACE_OUTER_BOUND('',#2269,.T.);
#1604=FACE_OUTER_BOUND('',#2270,.T.);
#1605=FACE_OUTER_BOUND('',#2271,.T.);
#1606=FACE_OUTER_BOUND('',#2273,.T.);
#1607=FACE_OUTER_BOUND('',#2274,.T.);
#1608=FACE_OUTER_BOUND('',#2275,.T.);
#1609=FACE_OUTER_BOUND('',#2276,.T.);
#1610=FACE_OUTER_BOUND('',#2277,.T.);
#1611=FACE_OUTER_BOUND('',#2278,.T.);
#1612=FACE_OUTER_BOUND('',#2279,.T.);
#1613=FACE_OUTER_BOUND('',#2281,.T.);
#1614=FACE_OUTER_BOUND('',#2282,.T.);
#1615=FACE_OUTER_BOUND('',#2283,.T.);
#1616=FACE_OUTER_BOUND('',#2284,.T.);
#1617=FACE_OUTER_BOUND('',#2285,.T.);
#1618=FACE_OUTER_BOUND('',#2286,.T.);
#1619=FACE_OUTER_BOUND('',#2287,.T.);
#1620=FACE_OUTER_BOUND('',#2288,.T.);
#1621=FACE_OUTER_BOUND('',#2289,.T.);
#1622=FACE_OUTER_BOUND('',#2291,.T.);
#1623=FACE_OUTER_BOUND('',#2292,.T.);
#1624=FACE_OUTER_BOUND('',#2293,.T.);
#1625=FACE_OUTER_BOUND('',#2294,.T.);
#1626=FACE_OUTER_BOUND('',#2295,.T.);
#1627=FACE_OUTER_BOUND('',#2296,.T.);
#1628=FACE_OUTER_BOUND('',#2297,.T.);
#1629=FACE_OUTER_BOUND('',#2299,.T.);
#1630=FACE_OUTER_BOUND('',#2300,.T.);
#1631=FACE_OUTER_BOUND('',#2301,.T.);
#1632=FACE_OUTER_BOUND('',#2302,.T.);
#1633=FACE_OUTER_BOUND('',#2303,.T.);
#1634=FACE_OUTER_BOUND('',#2304,.T.);
#1635=FACE_OUTER_BOUND('',#2305,.T.);
#1636=FACE_OUTER_BOUND('',#2306,.T.);
#1637=FACE_OUTER_BOUND('',#2307,.T.);
#1638=FACE_OUTER_BOUND('',#2308,.T.);
#1639=FACE_OUTER_BOUND('',#2309,.T.);
#1640=FACE_OUTER_BOUND('',#2310,.T.);
#1641=FACE_OUTER_BOUND('',#2311,.T.);
#1642=FACE_OUTER_BOUND('',#2312,.T.);
#1643=FACE_OUTER_BOUND('',#2314,.T.);
#1644=FACE_OUTER_BOUND('',#2316,.T.);
#1645=FACE_OUTER_BOUND('',#2318,.T.);
#1646=FACE_OUTER_BOUND('',#2319,.T.);
#1647=FACE_OUTER_BOUND('',#2320,.T.);
#1648=FACE_OUTER_BOUND('',#2321,.T.);
#1649=FACE_OUTER_BOUND('',#2322,.T.);
#1650=FACE_OUTER_BOUND('',#2323,.T.);
#1651=FACE_OUTER_BOUND('',#2325,.T.);
#1652=FACE_OUTER_BOUND('',#2326,.T.);
#1653=FACE_OUTER_BOUND('',#2329,.T.);
#1654=FACE_OUTER_BOUND('',#2330,.T.);
#1655=FACE_OUTER_BOUND('',#2332,.T.);
#1656=FACE_OUTER_BOUND('',#2333,.T.);
#1657=FACE_OUTER_BOUND('',#2335,.T.);
#1658=FACE_OUTER_BOUND('',#2336,.T.);
#1659=FACE_OUTER_BOUND('',#2338,.T.);
#1660=FACE_OUTER_BOUND('',#2339,.T.);
#1661=FACE_OUTER_BOUND('',#2341,.T.);
#1662=FACE_OUTER_BOUND('',#2342,.T.);
#1663=FACE_OUTER_BOUND('',#2343,.T.);
#1664=FACE_OUTER_BOUND('',#2344,.T.);
#1665=FACE_OUTER_BOUND('',#2345,.T.);
#1666=FACE_OUTER_BOUND('',#2346,.T.);
#1667=FACE_OUTER_BOUND('',#2347,.T.);
#1668=FACE_OUTER_BOUND('',#2348,.T.);
#1669=FACE_OUTER_BOUND('',#2349,.T.);
#1670=FACE_OUTER_BOUND('',#2350,.T.);
#1671=FACE_OUTER_BOUND('',#2351,.T.);
#1672=FACE_OUTER_BOUND('',#2352,.T.);
#1673=FACE_OUTER_BOUND('',#2353,.T.);
#1674=FACE_OUTER_BOUND('',#2354,.T.);
#1675=FACE_OUTER_BOUND('',#2356,.T.);
#1676=FACE_OUTER_BOUND('',#2357,.T.);
#1677=FACE_OUTER_BOUND('',#2358,.T.);
#1678=FACE_OUTER_BOUND('',#2359,.T.);
#1679=FACE_OUTER_BOUND('',#2360,.T.);
#1680=FACE_OUTER_BOUND('',#2361,.T.);
#1681=FACE_OUTER_BOUND('',#2362,.T.);
#1682=FACE_OUTER_BOUND('',#2364,.T.);
#1683=FACE_OUTER_BOUND('',#2365,.T.);
#1684=FACE_OUTER_BOUND('',#2366,.T.);
#1685=FACE_OUTER_BOUND('',#2367,.T.);
#1686=FACE_OUTER_BOUND('',#2368,.T.);
#1687=FACE_OUTER_BOUND('',#2369,.T.);
#1688=FACE_OUTER_BOUND('',#2370,.T.);
#1689=FACE_OUTER_BOUND('',#2371,.T.);
#1690=FACE_OUTER_BOUND('',#2372,.T.);
#1691=FACE_OUTER_BOUND('',#2373,.T.);
#1692=FACE_OUTER_BOUND('',#2374,.T.);
#1693=FACE_OUTER_BOUND('',#2375,.T.);
#1694=FACE_OUTER_BOUND('',#2376,.T.);
#1695=FACE_OUTER_BOUND('',#2377,.T.);
#1696=FACE_OUTER_BOUND('',#2378,.T.);
#1697=FACE_OUTER_BOUND('',#2379,.T.);
#1698=FACE_OUTER_BOUND('',#2380,.T.);
#1699=FACE_OUTER_BOUND('',#2381,.T.);
#1700=FACE_OUTER_BOUND('',#2382,.T.);
#1701=FACE_OUTER_BOUND('',#2383,.T.);
#1702=FACE_OUTER_BOUND('',#2384,.T.);
#1703=FACE_OUTER_BOUND('',#2385,.T.);
#1704=FACE_OUTER_BOUND('',#2386,.T.);
#1705=FACE_OUTER_BOUND('',#2387,.T.);
#1706=FACE_OUTER_BOUND('',#2388,.T.);
#1707=FACE_OUTER_BOUND('',#2389,.T.);
#1708=FACE_OUTER_BOUND('',#2390,.T.);
#1709=FACE_OUTER_BOUND('',#2391,.T.);
#1710=FACE_OUTER_BOUND('',#2392,.T.);
#1711=FACE_OUTER_BOUND('',#2393,.T.);
#1712=FACE_OUTER_BOUND('',#2394,.T.);
#1713=FACE_OUTER_BOUND('',#2395,.T.);
#1714=FACE_OUTER_BOUND('',#2396,.T.);
#1715=FACE_OUTER_BOUND('',#2397,.T.);
#1716=FACE_OUTER_BOUND('',#2398,.T.);
#1717=FACE_OUTER_BOUND('',#2399,.T.);
#1718=FACE_OUTER_BOUND('',#2400,.T.);
#1719=FACE_OUTER_BOUND('',#2401,.T.);
#1720=FACE_OUTER_BOUND('',#2402,.T.);
#1721=FACE_OUTER_BOUND('',#2403,.T.);
#1722=FACE_OUTER_BOUND('',#2404,.T.);
#1723=FACE_OUTER_BOUND('',#2429,.T.);
#1724=FACE_OUTER_BOUND('',#2454,.T.);
#1725=FACE_OUTER_BOUND('',#2455,.T.);
#1726=FACE_OUTER_BOUND('',#2456,.T.);
#1727=FACE_OUTER_BOUND('',#2457,.T.);
#1728=FACE_OUTER_BOUND('',#2458,.T.);
#1729=FACE_OUTER_BOUND('',#2459,.T.);
#1730=FACE_OUTER_BOUND('',#2460,.T.);
#1731=FACE_OUTER_BOUND('',#2461,.T.);
#1732=FACE_OUTER_BOUND('',#2462,.T.);
#1733=FACE_OUTER_BOUND('',#2463,.T.);
#1734=FACE_OUTER_BOUND('',#2464,.T.);
#1735=FACE_OUTER_BOUND('',#2466,.T.);
#1736=FACE_OUTER_BOUND('',#2468,.T.);
#1737=FACE_OUTER_BOUND('',#2469,.T.);
#1738=FACE_OUTER_BOUND('',#2470,.T.);
#1739=FACE_OUTER_BOUND('',#2476,.T.);
#1740=FACE_OUTER_BOUND('',#2478,.T.);
#1741=FACE_OUTER_BOUND('',#2479,.T.);
#1742=FACE_OUTER_BOUND('',#2480,.T.);
#1743=FACE_OUTER_BOUND('',#2481,.T.);
#1744=FACE_OUTER_BOUND('',#2482,.T.);
#1745=FACE_OUTER_BOUND('',#2483,.T.);
#1746=FACE_OUTER_BOUND('',#2484,.T.);
#1747=FACE_OUTER_BOUND('',#2485,.T.);
#1748=FACE_OUTER_BOUND('',#2486,.T.);
#1749=FACE_OUTER_BOUND('',#2487,.T.);
#1750=FACE_OUTER_BOUND('',#2488,.T.);
#1751=FACE_OUTER_BOUND('',#2490,.T.);
#1752=FACE_OUTER_BOUND('',#2492,.T.);
#1753=FACE_OUTER_BOUND('',#2493,.T.);
#1754=FACE_OUTER_BOUND('',#2494,.T.);
#1755=FACE_OUTER_BOUND('',#2500,.T.);
#1756=FACE_OUTER_BOUND('',#2502,.T.);
#1757=FACE_OUTER_BOUND('',#2503,.T.);
#1758=FACE_OUTER_BOUND('',#2504,.T.);
#1759=FACE_OUTER_BOUND('',#2505,.T.);
#1760=FACE_OUTER_BOUND('',#2506,.T.);
#1761=FACE_OUTER_BOUND('',#2507,.T.);
#1762=FACE_OUTER_BOUND('',#2508,.T.);
#1763=FACE_OUTER_BOUND('',#2509,.T.);
#1764=FACE_OUTER_BOUND('',#2510,.T.);
#1765=FACE_OUTER_BOUND('',#2511,.T.);
#1766=FACE_OUTER_BOUND('',#2512,.T.);
#1767=FACE_OUTER_BOUND('',#2514,.T.);
#1768=FACE_OUTER_BOUND('',#2516,.T.);
#1769=FACE_OUTER_BOUND('',#2517,.T.);
#1770=FACE_OUTER_BOUND('',#2518,.T.);
#1771=FACE_OUTER_BOUND('',#2524,.T.);
#1772=FACE_OUTER_BOUND('',#2526,.T.);
#1773=FACE_OUTER_BOUND('',#2527,.T.);
#1774=FACE_OUTER_BOUND('',#2528,.T.);
#1775=FACE_OUTER_BOUND('',#2529,.T.);
#1776=FACE_OUTER_BOUND('',#2530,.T.);
#1777=FACE_OUTER_BOUND('',#2531,.T.);
#1778=FACE_OUTER_BOUND('',#2532,.T.);
#1779=FACE_OUTER_BOUND('',#2533,.T.);
#1780=FACE_OUTER_BOUND('',#2534,.T.);
#1781=FACE_OUTER_BOUND('',#2535,.T.);
#1782=FACE_OUTER_BOUND('',#2536,.T.);
#1783=FACE_OUTER_BOUND('',#2538,.T.);
#1784=FACE_OUTER_BOUND('',#2540,.T.);
#1785=FACE_OUTER_BOUND('',#2541,.T.);
#1786=FACE_OUTER_BOUND('',#2542,.T.);
#1787=FACE_OUTER_BOUND('',#2548,.T.);
#1788=FACE_OUTER_BOUND('',#2550,.T.);
#1789=FACE_OUTER_BOUND('',#2551,.T.);
#1790=FACE_OUTER_BOUND('',#2552,.T.);
#1791=FACE_OUTER_BOUND('',#2553,.T.);
#1792=FACE_OUTER_BOUND('',#2554,.T.);
#1793=FACE_OUTER_BOUND('',#2560,.T.);
#1794=FACE_OUTER_BOUND('',#2561,.T.);
#1795=FACE_OUTER_BOUND('',#2562,.T.);
#1796=FACE_OUTER_BOUND('',#2567,.T.);
#1797=FACE_OUTER_BOUND('',#2568,.T.);
#1798=FACE_OUTER_BOUND('',#2569,.T.);
#1799=FACE_OUTER_BOUND('',#2570,.T.);
#1800=FACE_OUTER_BOUND('',#2571,.T.);
#1801=FACE_OUTER_BOUND('',#2572,.T.);
#1802=FACE_OUTER_BOUND('',#2573,.T.);
#1803=FACE_OUTER_BOUND('',#2575,.T.);
#1804=FACE_OUTER_BOUND('',#2576,.T.);
#1805=FACE_OUTER_BOUND('',#2578,.T.);
#1806=FACE_OUTER_BOUND('',#2579,.T.);
#1807=FACE_OUTER_BOUND('',#2581,.T.);
#1808=FACE_OUTER_BOUND('',#2582,.T.);
#1809=FACE_OUTER_BOUND('',#2584,.T.);
#1810=FACE_OUTER_BOUND('',#2585,.T.);
#1811=FACE_OUTER_BOUND('',#2587,.T.);
#1812=FACE_OUTER_BOUND('',#2588,.T.);
#1813=FACE_OUTER_BOUND('',#2590,.T.);
#1814=FACE_OUTER_BOUND('',#2592,.T.);
#1815=FACE_OUTER_BOUND('',#2593,.T.);
#1816=FACE_OUTER_BOUND('',#2594,.T.);
#1817=FACE_OUTER_BOUND('',#2595,.T.);
#1818=FACE_OUTER_BOUND('',#2596,.T.);
#1819=FACE_OUTER_BOUND('',#2598,.T.);
#1820=FACE_OUTER_BOUND('',#2600,.T.);
#1821=FACE_OUTER_BOUND('',#2602,.T.);
#1822=FACE_OUTER_BOUND('',#2604,.T.);
#1823=FACE_OUTER_BOUND('',#2605,.T.);
#1824=FACE_OUTER_BOUND('',#2606,.T.);
#1825=FACE_OUTER_BOUND('',#2607,.T.);
#1826=FACE_OUTER_BOUND('',#2608,.T.);
#1827=FACE_OUTER_BOUND('',#2610,.T.);
#1828=FACE_OUTER_BOUND('',#2611,.T.);
#1829=FACE_OUTER_BOUND('',#2612,.T.);
#1830=FACE_OUTER_BOUND('',#2613,.T.);
#1831=FACE_OUTER_BOUND('',#2614,.T.);
#1832=FACE_OUTER_BOUND('',#2615,.T.);
#1833=FACE_OUTER_BOUND('',#2616,.T.);
#1834=FACE_OUTER_BOUND('',#2617,.T.);
#1835=FACE_OUTER_BOUND('',#2618,.T.);
#1836=FACE_OUTER_BOUND('',#2619,.T.);
#1837=FACE_OUTER_BOUND('',#2620,.T.);
#1838=FACE_OUTER_BOUND('',#2621,.T.);
#1839=EDGE_LOOP('',(#6246,#6247,#6248,#6249));
#1840=EDGE_LOOP('',(#6250,#6251,#6252,#6253));
#1841=EDGE_LOOP('',(#6254,#6255,#6256,#6257));
#1842=EDGE_LOOP('',(#6258,#6259,#6260,#6261));
#1843=EDGE_LOOP('',(#6262,#6263,#6264,#6265));
#1844=EDGE_LOOP('',(#6266,#6267,#6268,#6269));
#1845=EDGE_LOOP('',(#6270,#6271,#6272,#6273));
#1846=EDGE_LOOP('',(#6274,#6275,#6276,#6277));
#1847=EDGE_LOOP('',(#6278,#6279,#6280,#6281));
#1848=EDGE_LOOP('',(#6282,#6283,#6284,#6285));
#1849=EDGE_LOOP('',(#6286,#6287,#6288,#6289));
#1850=EDGE_LOOP('',(#6290,#6291,#6292,#6293));
#1851=EDGE_LOOP('',(#6294,#6295,#6296,#6297));
#1852=EDGE_LOOP('',(#6298,#6299,#6300,#6301));
#1853=EDGE_LOOP('',(#6302,#6303,#6304,#6305));
#1854=EDGE_LOOP('',(#6306,#6307,#6308,#6309));
#1855=EDGE_LOOP('',(#6310,#6311,#6312,#6313));
#1856=EDGE_LOOP('',(#6314,#6315,#6316,#6317));
#1857=EDGE_LOOP('',(#6318,#6319,#6320,#6321));
#1858=EDGE_LOOP('',(#6322,#6323,#6324,#6325));
#1859=EDGE_LOOP('',(#6326,#6327,#6328,#6329));
#1860=EDGE_LOOP('',(#6330,#6331,#6332,#6333));
#1861=EDGE_LOOP('',(#6334,#6335,#6336,#6337));
#1862=EDGE_LOOP('',(#6338,#6339,#6340,#6341));
#1863=EDGE_LOOP('',(#6342,#6343,#6344,#6345));
#1864=EDGE_LOOP('',(#6346,#6347,#6348,#6349));
#1865=EDGE_LOOP('',(#6350,#6351,#6352,#6353));
#1866=EDGE_LOOP('',(#6354));
#1867=EDGE_LOOP('',(#6355));
#1868=EDGE_LOOP('',(#6356));
#1869=EDGE_LOOP('',(#6357));
#1870=EDGE_LOOP('',(#6358));
#1871=EDGE_LOOP('',(#6359));
#1872=EDGE_LOOP('',(#6360));
#1873=EDGE_LOOP('',(#6361));
#1874=EDGE_LOOP('',(#6362));
#1875=EDGE_LOOP('',(#6363));
#1876=EDGE_LOOP('',(#6364));
#1877=EDGE_LOOP('',(#6365));
#1878=EDGE_LOOP('',(#6366));
#1879=EDGE_LOOP('',(#6367));
#1880=EDGE_LOOP('',(#6368));
#1881=EDGE_LOOP('',(#6369));
#1882=EDGE_LOOP('',(#6370));
#1883=EDGE_LOOP('',(#6371));
#1884=EDGE_LOOP('',(#6372));
#1885=EDGE_LOOP('',(#6373));
#1886=EDGE_LOOP('',(#6374));
#1887=EDGE_LOOP('',(#6375));
#1888=EDGE_LOOP('',(#6376,#6377,#6378,#6379));
#1889=EDGE_LOOP('',(#6380));
#1890=EDGE_LOOP('',(#6381));
#1891=EDGE_LOOP('',(#6382));
#1892=EDGE_LOOP('',(#6383));
#1893=EDGE_LOOP('',(#6384));
#1894=EDGE_LOOP('',(#6385));
#1895=EDGE_LOOP('',(#6386));
#1896=EDGE_LOOP('',(#6387));
#1897=EDGE_LOOP('',(#6388));
#1898=EDGE_LOOP('',(#6389));
#1899=EDGE_LOOP('',(#6390));
#1900=EDGE_LOOP('',(#6391));
#1901=EDGE_LOOP('',(#6392));
#1902=EDGE_LOOP('',(#6393));
#1903=EDGE_LOOP('',(#6394));
#1904=EDGE_LOOP('',(#6395));
#1905=EDGE_LOOP('',(#6396));
#1906=EDGE_LOOP('',(#6397));
#1907=EDGE_LOOP('',(#6398));
#1908=EDGE_LOOP('',(#6399));
#1909=EDGE_LOOP('',(#6400));
#1910=EDGE_LOOP('',(#6401));
#1911=EDGE_LOOP('',(#6402,#6403,#6404,#6405));
#1912=EDGE_LOOP('',(#6406,#6407,#6408,#6409));
#1913=EDGE_LOOP('',(#6410,#6411,#6412,#6413));
#1914=EDGE_LOOP('',(#6414,#6415,#6416,#6417));
#1915=EDGE_LOOP('',(#6418,#6419,#6420,#6421));
#1916=EDGE_LOOP('',(#6422,#6423,#6424,#6425));
#1917=EDGE_LOOP('',(#6426,#6427,#6428,#6429));
#1918=EDGE_LOOP('',(#6430,#6431,#6432,#6433));
#1919=EDGE_LOOP('',(#6434,#6435,#6436,#6437));
#1920=EDGE_LOOP('',(#6438,#6439,#6440,#6441));
#1921=EDGE_LOOP('',(#6442,#6443,#6444,#6445));
#1922=EDGE_LOOP('',(#6446,#6447,#6448,#6449));
#1923=EDGE_LOOP('',(#6450,#6451,#6452,#6453));
#1924=EDGE_LOOP('',(#6454,#6455,#6456,#6457));
#1925=EDGE_LOOP('',(#6458,#6459,#6460,#6461));
#1926=EDGE_LOOP('',(#6462,#6463,#6464,#6465));
#1927=EDGE_LOOP('',(#6466,#6467,#6468,#6469));
#1928=EDGE_LOOP('',(#6470,#6471,#6472,#6473));
#1929=EDGE_LOOP('',(#6474,#6475,#6476,#6477));
#1930=EDGE_LOOP('',(#6478,#6479,#6480,#6481));
#1931=EDGE_LOOP('',(#6482,#6483,#6484,#6485));
#1932=EDGE_LOOP('',(#6486,#6487,#6488,#6489));
#1933=EDGE_LOOP('',(#6490,#6491,#6492,#6493));
#1934=EDGE_LOOP('',(#6494,#6495,#6496,#6497));
#1935=EDGE_LOOP('',(#6498,#6499,#6500,#6501));
#1936=EDGE_LOOP('',(#6502,#6503,#6504,#6505));
#1937=EDGE_LOOP('',(#6506,#6507,#6508,#6509));
#1938=EDGE_LOOP('',(#6510,#6511,#6512,#6513));
#1939=EDGE_LOOP('',(#6514,#6515,#6516,#6517));
#1940=EDGE_LOOP('',(#6518,#6519,#6520,#6521));
#1941=EDGE_LOOP('',(#6522,#6523,#6524,#6525));
#1942=EDGE_LOOP('',(#6526,#6527,#6528,#6529));
#1943=EDGE_LOOP('',(#6530,#6531,#6532,#6533));
#1944=EDGE_LOOP('',(#6534,#6535,#6536,#6537));
#1945=EDGE_LOOP('',(#6538,#6539,#6540,#6541));
#1946=EDGE_LOOP('',(#6542));
#1947=EDGE_LOOP('',(#6543));
#1948=EDGE_LOOP('',(#6544));
#1949=EDGE_LOOP('',(#6545));
#1950=EDGE_LOOP('',(#6546));
#1951=EDGE_LOOP('',(#6547));
#1952=EDGE_LOOP('',(#6548));
#1953=EDGE_LOOP('',(#6549));
#1954=EDGE_LOOP('',(#6550));
#1955=EDGE_LOOP('',(#6551));
#1956=EDGE_LOOP('',(#6552));
#1957=EDGE_LOOP('',(#6553));
#1958=EDGE_LOOP('',(#6554));
#1959=EDGE_LOOP('',(#6555));
#1960=EDGE_LOOP('',(#6556));
#1961=EDGE_LOOP('',(#6557));
#1962=EDGE_LOOP('',(#6558));
#1963=EDGE_LOOP('',(#6559));
#1964=EDGE_LOOP('',(#6560,#6561,#6562,#6563));
#1965=EDGE_LOOP('',(#6564));
#1966=EDGE_LOOP('',(#6565));
#1967=EDGE_LOOP('',(#6566));
#1968=EDGE_LOOP('',(#6567));
#1969=EDGE_LOOP('',(#6568));
#1970=EDGE_LOOP('',(#6569));
#1971=EDGE_LOOP('',(#6570));
#1972=EDGE_LOOP('',(#6571));
#1973=EDGE_LOOP('',(#6572));
#1974=EDGE_LOOP('',(#6573));
#1975=EDGE_LOOP('',(#6574));
#1976=EDGE_LOOP('',(#6575));
#1977=EDGE_LOOP('',(#6576));
#1978=EDGE_LOOP('',(#6577));
#1979=EDGE_LOOP('',(#6578));
#1980=EDGE_LOOP('',(#6579));
#1981=EDGE_LOOP('',(#6580));
#1982=EDGE_LOOP('',(#6581));
#1983=EDGE_LOOP('',(#6582,#6583,#6584,#6585));
#1984=EDGE_LOOP('',(#6586));
#1985=EDGE_LOOP('',(#6587,#6588,#6589,#6590));
#1986=EDGE_LOOP('',(#6591));
#1987=EDGE_LOOP('',(#6592,#6593,#6594,#6595));
#1988=EDGE_LOOP('',(#6596));
#1989=EDGE_LOOP('',(#6597,#6598,#6599,#6600));
#1990=EDGE_LOOP('',(#6601));
#1991=EDGE_LOOP('',(#6602,#6603,#6604,#6605));
#1992=EDGE_LOOP('',(#6606,#6607,#6608,#6609));
#1993=EDGE_LOOP('',(#6610,#6611,#6612,#6613));
#1994=EDGE_LOOP('',(#6614,#6615,#6616,#6617));
#1995=EDGE_LOOP('',(#6618,#6619,#6620,#6621));
#1996=EDGE_LOOP('',(#6622));
#1997=EDGE_LOOP('',(#6623));
#1998=EDGE_LOOP('',(#6624,#6625,#6626,#6627));
#1999=EDGE_LOOP('',(#6628));
#2000=EDGE_LOOP('',(#6629));
#2001=EDGE_LOOP('',(#6630,#6631,#6632,#6633));
#2002=EDGE_LOOP('',(#6634));
#2003=EDGE_LOOP('',(#6635,#6636,#6637,#6638));
#2004=EDGE_LOOP('',(#6639));
#2005=EDGE_LOOP('',(#6640,#6641,#6642,#6643));
#2006=EDGE_LOOP('',(#6644));
#2007=EDGE_LOOP('',(#6645,#6646,#6647,#6648));
#2008=EDGE_LOOP('',(#6649));
#2009=EDGE_LOOP('',(#6650,#6651,#6652,#6653));
#2010=EDGE_LOOP('',(#6654,#6655,#6656,#6657));
#2011=EDGE_LOOP('',(#6658,#6659,#6660,#6661));
#2012=EDGE_LOOP('',(#6662,#6663,#6664,#6665));
#2013=EDGE_LOOP('',(#6666,#6667,#6668,#6669));
#2014=EDGE_LOOP('',(#6670));
#2015=EDGE_LOOP('',(#6671));
#2016=EDGE_LOOP('',(#6672,#6673,#6674,#6675));
#2017=EDGE_LOOP('',(#6676));
#2018=EDGE_LOOP('',(#6677));
#2019=EDGE_LOOP('',(#6678,#6679,#6680,#6681));
#2020=EDGE_LOOP('',(#6682));
#2021=EDGE_LOOP('',(#6683,#6684,#6685,#6686));
#2022=EDGE_LOOP('',(#6687));
#2023=EDGE_LOOP('',(#6688,#6689,#6690,#6691));
#2024=EDGE_LOOP('',(#6692,#6693,#6694,#6695));
#2025=EDGE_LOOP('',(#6696,#6697,#6698,#6699));
#2026=EDGE_LOOP('',(#6700));
#2027=EDGE_LOOP('',(#6701));
#2028=EDGE_LOOP('',(#6702,#6703,#6704,#6705));
#2029=EDGE_LOOP('',(#6706,#6707,#6708,#6709));
#2030=EDGE_LOOP('',(#6710));
#2031=EDGE_LOOP('',(#6711));
#2032=EDGE_LOOP('',(#6712,#6713,#6714,#6715));
#2033=EDGE_LOOP('',(#6716,#6717,#6718,#6719));
#2034=EDGE_LOOP('',(#6720,#6721,#6722,#6723));
#2035=EDGE_LOOP('',(#6724));
#2036=EDGE_LOOP('',(#6725));
#2037=EDGE_LOOP('',(#6726,#6727,#6728,#6729));
#2038=EDGE_LOOP('',(#6730,#6731,#6732,#6733));
#2039=EDGE_LOOP('',(#6734,#6735,#6736,#6737,#6738,#6739,#6740,#6741));
#2040=EDGE_LOOP('',(#6742,#6743,#6744));
#2041=EDGE_LOOP('',(#6745,#6746,#6747,#6748,#6749,#6750,#6751,#6752));
#2042=EDGE_LOOP('',(#6753,#6754,#6755));
#2043=EDGE_LOOP('',(#6756,#6757,#6758,#6759,#6760,#6761,#6762,#6763));
#2044=EDGE_LOOP('',(#6764,#6765,#6766,#6767,#6768,#6769,#6770,#6771,#6772,
#6773,#6774,#6775));
#2045=EDGE_LOOP('',(#6776));
#2046=EDGE_LOOP('',(#6777));
#2047=EDGE_LOOP('',(#6778,#6779,#6780,#6781));
#2048=EDGE_LOOP('',(#6782,#6783,#6784,#6785,#6786,#6787));
#2049=EDGE_LOOP('',(#6788,#6789,#6790,#6791));
#2050=EDGE_LOOP('',(#6792));
#2051=EDGE_LOOP('',(#6793));
#2052=EDGE_LOOP('',(#6794,#6795,#6796,#6797,#6798,#6799));
#2053=EDGE_LOOP('',(#6800,#6801,#6802,#6803));
#2054=EDGE_LOOP('',(#6804));
#2055=EDGE_LOOP('',(#6805));
#2056=EDGE_LOOP('',(#6806,#6807,#6808,#6809));
#2057=EDGE_LOOP('',(#6810,#6811,#6812,#6813));
#2058=EDGE_LOOP('',(#6814,#6815,#6816,#6817));
#2059=EDGE_LOOP('',(#6818));
#2060=EDGE_LOOP('',(#6819));
#2061=EDGE_LOOP('',(#6820));
#2062=EDGE_LOOP('',(#6821));
#2063=EDGE_LOOP('',(#6822,#6823,#6824,#6825));
#2064=EDGE_LOOP('',(#6826));
#2065=EDGE_LOOP('',(#6827));
#2066=EDGE_LOOP('',(#6828,#6829,#6830,#6831));
#2067=EDGE_LOOP('',(#6832));
#2068=EDGE_LOOP('',(#6833,#6834,#6835,#6836));
#2069=EDGE_LOOP('',(#6837));
#2070=EDGE_LOOP('',(#6838,#6839,#6840,#6841));
#2071=EDGE_LOOP('',(#6842,#6843,#6844,#6845));
#2072=EDGE_LOOP('',(#6846,#6847,#6848,#6849));
#2073=EDGE_LOOP('',(#6850));
#2074=EDGE_LOOP('',(#6851));
#2075=EDGE_LOOP('',(#6852,#6853,#6854,#6855));
#2076=EDGE_LOOP('',(#6856,#6857,#6858,#6859));
#2077=EDGE_LOOP('',(#6860));
#2078=EDGE_LOOP('',(#6861));
#2079=EDGE_LOOP('',(#6862,#6863,#6864,#6865));
#2080=EDGE_LOOP('',(#6866,#6867,#6868,#6869));
#2081=EDGE_LOOP('',(#6870,#6871,#6872,#6873));
#2082=EDGE_LOOP('',(#6874));
#2083=EDGE_LOOP('',(#6875));
#2084=EDGE_LOOP('',(#6876,#6877,#6878,#6879));
#2085=EDGE_LOOP('',(#6880,#6881,#6882,#6883));
#2086=EDGE_LOOP('',(#6884,#6885,#6886,#6887,#6888,#6889,#6890,#6891));
#2087=EDGE_LOOP('',(#6892,#6893,#6894));
#2088=EDGE_LOOP('',(#6895,#6896,#6897,#6898,#6899,#6900,#6901,#6902));
#2089=EDGE_LOOP('',(#6903,#6904,#6905));
#2090=EDGE_LOOP('',(#6906,#6907,#6908,#6909,#6910,#6911,#6912,#6913));
#2091=EDGE_LOOP('',(#6914,#6915,#6916,#6917,#6918,#6919,#6920,#6921,#6922,
#6923,#6924,#6925));
#2092=EDGE_LOOP('',(#6926));
#2093=EDGE_LOOP('',(#6927));
#2094=EDGE_LOOP('',(#6928,#6929,#6930,#6931));
#2095=EDGE_LOOP('',(#6932,#6933,#6934,#6935,#6936,#6937));
#2096=EDGE_LOOP('',(#6938,#6939,#6940,#6941));
#2097=EDGE_LOOP('',(#6942));
#2098=EDGE_LOOP('',(#6943));
#2099=EDGE_LOOP('',(#6944,#6945,#6946,#6947,#6948,#6949));
#2100=EDGE_LOOP('',(#6950,#6951,#6952,#6953));
#2101=EDGE_LOOP('',(#6954));
#2102=EDGE_LOOP('',(#6955));
#2103=EDGE_LOOP('',(#6956,#6957,#6958,#6959));
#2104=EDGE_LOOP('',(#6960,#6961,#6962,#6963));
#2105=EDGE_LOOP('',(#6964,#6965,#6966,#6967));
#2106=EDGE_LOOP('',(#6968));
#2107=EDGE_LOOP('',(#6969));
#2108=EDGE_LOOP('',(#6970));
#2109=EDGE_LOOP('',(#6971));
#2110=EDGE_LOOP('',(#6972,#6973,#6974,#6975));
#2111=EDGE_LOOP('',(#6976));
#2112=EDGE_LOOP('',(#6977));
#2113=EDGE_LOOP('',(#6978,#6979,#6980,#6981));
#2114=EDGE_LOOP('',(#6982));
#2115=EDGE_LOOP('',(#6983,#6984,#6985,#6986));
#2116=EDGE_LOOP('',(#6987));
#2117=EDGE_LOOP('',(#6988,#6989,#6990,#6991));
#2118=EDGE_LOOP('',(#6992,#6993,#6994,#6995));
#2119=EDGE_LOOP('',(#6996,#6997,#6998,#6999));
#2120=EDGE_LOOP('',(#7000));
#2121=EDGE_LOOP('',(#7001));
#2122=EDGE_LOOP('',(#7002,#7003,#7004,#7005));
#2123=EDGE_LOOP('',(#7006,#7007,#7008,#7009));
#2124=EDGE_LOOP('',(#7010));
#2125=EDGE_LOOP('',(#7011));
#2126=EDGE_LOOP('',(#7012,#7013,#7014,#7015));
#2127=EDGE_LOOP('',(#7016,#7017,#7018,#7019));
#2128=EDGE_LOOP('',(#7020,#7021,#7022,#7023));
#2129=EDGE_LOOP('',(#7024));
#2130=EDGE_LOOP('',(#7025));
#2131=EDGE_LOOP('',(#7026,#7027,#7028,#7029));
#2132=EDGE_LOOP('',(#7030,#7031,#7032,#7033));
#2133=EDGE_LOOP('',(#7034,#7035,#7036,#7037,#7038,#7039,#7040,#7041));
#2134=EDGE_LOOP('',(#7042,#7043,#7044));
#2135=EDGE_LOOP('',(#7045,#7046,#7047,#7048,#7049,#7050,#7051,#7052));
#2136=EDGE_LOOP('',(#7053,#7054,#7055));
#2137=EDGE_LOOP('',(#7056,#7057,#7058,#7059,#7060,#7061,#7062,#7063));
#2138=EDGE_LOOP('',(#7064,#7065,#7066,#7067,#7068,#7069,#7070,#7071,#7072,
#7073,#7074,#7075));
#2139=EDGE_LOOP('',(#7076));
#2140=EDGE_LOOP('',(#7077));
#2141=EDGE_LOOP('',(#7078,#7079,#7080,#7081));
#2142=EDGE_LOOP('',(#7082,#7083,#7084,#7085,#7086,#7087));
#2143=EDGE_LOOP('',(#7088,#7089,#7090,#7091));
#2144=EDGE_LOOP('',(#7092));
#2145=EDGE_LOOP('',(#7093));
#2146=EDGE_LOOP('',(#7094,#7095,#7096,#7097,#7098,#7099));
#2147=EDGE_LOOP('',(#7100,#7101,#7102,#7103));
#2148=EDGE_LOOP('',(#7104));
#2149=EDGE_LOOP('',(#7105));
#2150=EDGE_LOOP('',(#7106,#7107,#7108,#7109));
#2151=EDGE_LOOP('',(#7110,#7111,#7112,#7113));
#2152=EDGE_LOOP('',(#7114,#7115,#7116,#7117));
#2153=EDGE_LOOP('',(#7118));
#2154=EDGE_LOOP('',(#7119));
#2155=EDGE_LOOP('',(#7120));
#2156=EDGE_LOOP('',(#7121));
#2157=EDGE_LOOP('',(#7122,#7123,#7124,#7125));
#2158=EDGE_LOOP('',(#7126));
#2159=EDGE_LOOP('',(#7127));
#2160=EDGE_LOOP('',(#7128,#7129,#7130,#7131));
#2161=EDGE_LOOP('',(#7132));
#2162=EDGE_LOOP('',(#7133,#7134,#7135,#7136));
#2163=EDGE_LOOP('',(#7137));
#2164=EDGE_LOOP('',(#7138,#7139,#7140,#7141));
#2165=EDGE_LOOP('',(#7142,#7143,#7144,#7145));
#2166=EDGE_LOOP('',(#7146,#7147,#7148,#7149));
#2167=EDGE_LOOP('',(#7150));
#2168=EDGE_LOOP('',(#7151));
#2169=EDGE_LOOP('',(#7152,#7153,#7154,#7155));
#2170=EDGE_LOOP('',(#7156,#7157,#7158,#7159));
#2171=EDGE_LOOP('',(#7160));
#2172=EDGE_LOOP('',(#7161));
#2173=EDGE_LOOP('',(#7162,#7163,#7164,#7165));
#2174=EDGE_LOOP('',(#7166,#7167,#7168,#7169));
#2175=EDGE_LOOP('',(#7170,#7171,#7172,#7173));
#2176=EDGE_LOOP('',(#7174));
#2177=EDGE_LOOP('',(#7175));
#2178=EDGE_LOOP('',(#7176,#7177,#7178,#7179));
#2179=EDGE_LOOP('',(#7180,#7181,#7182,#7183));
#2180=EDGE_LOOP('',(#7184,#7185,#7186,#7187,#7188,#7189,#7190,#7191));
#2181=EDGE_LOOP('',(#7192,#7193,#7194));
#2182=EDGE_LOOP('',(#7195,#7196,#7197,#7198,#7199,#7200,#7201,#7202));
#2183=EDGE_LOOP('',(#7203,#7204,#7205));
#2184=EDGE_LOOP('',(#7206,#7207,#7208,#7209,#7210,#7211,#7212,#7213));
#2185=EDGE_LOOP('',(#7214,#7215,#7216,#7217,#7218,#7219,#7220,#7221,#7222,
#7223,#7224,#7225));
#2186=EDGE_LOOP('',(#7226));
#2187=EDGE_LOOP('',(#7227));
#2188=EDGE_LOOP('',(#7228,#7229,#7230,#7231));
#2189=EDGE_LOOP('',(#7232,#7233,#7234,#7235,#7236,#7237));
#2190=EDGE_LOOP('',(#7238,#7239,#7240,#7241));
#2191=EDGE_LOOP('',(#7242));
#2192=EDGE_LOOP('',(#7243));
#2193=EDGE_LOOP('',(#7244,#7245,#7246,#7247,#7248,#7249));
#2194=EDGE_LOOP('',(#7250,#7251,#7252,#7253));
#2195=EDGE_LOOP('',(#7254));
#2196=EDGE_LOOP('',(#7255));
#2197=EDGE_LOOP('',(#7256,#7257,#7258,#7259));
#2198=EDGE_LOOP('',(#7260,#7261,#7262,#7263));
#2199=EDGE_LOOP('',(#7264,#7265,#7266,#7267));
#2200=EDGE_LOOP('',(#7268));
#2201=EDGE_LOOP('',(#7269));
#2202=EDGE_LOOP('',(#7270));
#2203=EDGE_LOOP('',(#7271));
#2204=EDGE_LOOP('',(#7272,#7273,#7274,#7275));
#2205=EDGE_LOOP('',(#7276));
#2206=EDGE_LOOP('',(#7277));
#2207=EDGE_LOOP('',(#7278,#7279,#7280,#7281));
#2208=EDGE_LOOP('',(#7282));
#2209=EDGE_LOOP('',(#7283,#7284,#7285,#7286));
#2210=EDGE_LOOP('',(#7287));
#2211=EDGE_LOOP('',(#7288,#7289,#7290,#7291));
#2212=EDGE_LOOP('',(#7292));
#2213=EDGE_LOOP('',(#7293,#7294,#7295,#7296));
#2214=EDGE_LOOP('',(#7297));
#2215=EDGE_LOOP('',(#7298,#7299,#7300,#7301));
#2216=EDGE_LOOP('',(#7302));
#2217=EDGE_LOOP('',(#7303,#7304,#7305,#7306));
#2218=EDGE_LOOP('',(#7307));
#2219=EDGE_LOOP('',(#7308));
#2220=EDGE_LOOP('',(#7309,#7310,#7311,#7312));
#2221=EDGE_LOOP('',(#7313,#7314,#7315,#7316));
#2222=EDGE_LOOP('',(#7317,#7318,#7319,#7320));
#2223=EDGE_LOOP('',(#7321,#7322,#7323,#7324));
#2224=EDGE_LOOP('',(#7325,#7326,#7327,#7328));
#2225=EDGE_LOOP('',(#7329));
#2226=EDGE_LOOP('',(#7330,#7331,#7332,#7333));
#2227=EDGE_LOOP('',(#7334));
#2228=EDGE_LOOP('',(#7335));
#2229=EDGE_LOOP('',(#7336));
#2230=EDGE_LOOP('',(#7337));
#2231=EDGE_LOOP('',(#7338,#7339,#7340,#7341));
#2232=EDGE_LOOP('',(#7342,#7343,#7344,#7345));
#2233=EDGE_LOOP('',(#7346,#7347,#7348,#7349));
#2234=EDGE_LOOP('',(#7350,#7351,#7352,#7353));
#2235=EDGE_LOOP('',(#7354,#7355,#7356,#7357));
#2236=EDGE_LOOP('',(#7358,#7359,#7360,#7361));
#2237=EDGE_LOOP('',(#7362,#7363,#7364,#7365));
#2238=EDGE_LOOP('',(#7366,#7367,#7368,#7369));
#2239=EDGE_LOOP('',(#7370,#7371,#7372,#7373));
#2240=EDGE_LOOP('',(#7374,#7375,#7376,#7377));
#2241=EDGE_LOOP('',(#7378,#7379,#7380,#7381));
#2242=EDGE_LOOP('',(#7382,#7383,#7384,#7385));
#2243=EDGE_LOOP('',(#7386,#7387,#7388,#7389));
#2244=EDGE_LOOP('',(#7390));
#2245=EDGE_LOOP('',(#7391));
#2246=EDGE_LOOP('',(#7392));
#2247=EDGE_LOOP('',(#7393));
#2248=EDGE_LOOP('',(#7394));
#2249=EDGE_LOOP('',(#7395));
#2250=EDGE_LOOP('',(#7396));
#2251=EDGE_LOOP('',(#7397));
#2252=EDGE_LOOP('',(#7398,#7399,#7400,#7401));
#2253=EDGE_LOOP('',(#7402));
#2254=EDGE_LOOP('',(#7403));
#2255=EDGE_LOOP('',(#7404));
#2256=EDGE_LOOP('',(#7405));
#2257=EDGE_LOOP('',(#7406));
#2258=EDGE_LOOP('',(#7407));
#2259=EDGE_LOOP('',(#7408));
#2260=EDGE_LOOP('',(#7409));
#2261=EDGE_LOOP('',(#7410,#7411,#7412,#7413));
#2262=EDGE_LOOP('',(#7414,#7415,#7416,#7417));
#2263=EDGE_LOOP('',(#7418));
#2264=EDGE_LOOP('',(#7419));
#2265=EDGE_LOOP('',(#7420));
#2266=EDGE_LOOP('',(#7421));
#2267=EDGE_LOOP('',(#7422,#7423,#7424,#7425));
#2268=EDGE_LOOP('',(#7426));
#2269=EDGE_LOOP('',(#7427,#7428,#7429,#7430));
#2270=EDGE_LOOP('',(#7431));
#2271=EDGE_LOOP('',(#7432));
#2272=EDGE_LOOP('',(#7433));
#2273=EDGE_LOOP('',(#7434,#7435,#7436,#7437));
#2274=EDGE_LOOP('',(#7438));
#2275=EDGE_LOOP('',(#7439));
#2276=EDGE_LOOP('',(#7440,#7441,#7442,#7443));
#2277=EDGE_LOOP('',(#7444));
#2278=EDGE_LOOP('',(#7445,#7446,#7447,#7448));
#2279=EDGE_LOOP('',(#7449));
#2280=EDGE_LOOP('',(#7450));
#2281=EDGE_LOOP('',(#7451));
#2282=EDGE_LOOP('',(#7452,#7453,#7454,#7455));
#2283=EDGE_LOOP('',(#7456));
#2284=EDGE_LOOP('',(#7457));
#2285=EDGE_LOOP('',(#7458,#7459,#7460,#7461));
#2286=EDGE_LOOP('',(#7462));
#2287=EDGE_LOOP('',(#7463,#7464,#7465,#7466));
#2288=EDGE_LOOP('',(#7467));
#2289=EDGE_LOOP('',(#7468));
#2290=EDGE_LOOP('',(#7469));
#2291=EDGE_LOOP('',(#7470,#7471,#7472,#7473));
#2292=EDGE_LOOP('',(#7474));
#2293=EDGE_LOOP('',(#7475));
#2294=EDGE_LOOP('',(#7476,#7477,#7478,#7479));
#2295=EDGE_LOOP('',(#7480));
#2296=EDGE_LOOP('',(#7481,#7482,#7483,#7484));
#2297=EDGE_LOOP('',(#7485));
#2298=EDGE_LOOP('',(#7486));
#2299=EDGE_LOOP('',(#7487));
#2300=EDGE_LOOP('',(#7488,#7489,#7490,#7491));
#2301=EDGE_LOOP('',(#7492));
#2302=EDGE_LOOP('',(#7493));
#2303=EDGE_LOOP('',(#7494,#7495,#7496,#7497));
#2304=EDGE_LOOP('',(#7498,#7499,#7500,#7501));
#2305=EDGE_LOOP('',(#7502));
#2306=EDGE_LOOP('',(#7503,#7504,#7505,#7506));
#2307=EDGE_LOOP('',(#7507));
#2308=EDGE_LOOP('',(#7508,#7509));
#2309=EDGE_LOOP('',(#7510,#7511,#7512,#7513));
#2310=EDGE_LOOP('',(#7514,#7515,#7516,#7517));
#2311=EDGE_LOOP('',(#7518,#7519));
#2312=EDGE_LOOP('',(#7520,#7521,#7522,#7523,#7524,#7525));
#2313=EDGE_LOOP('',(#7526));
#2314=EDGE_LOOP('',(#7527,#7528,#7529,#7530,#7531,#7532,#7533,#7534));
#2315=EDGE_LOOP('',(#7535));
#2316=EDGE_LOOP('',(#7536,#7537,#7538,#7539,#7540,#7541));
#2317=EDGE_LOOP('',(#7542));
#2318=EDGE_LOOP('',(#7543,#7544,#7545,#7546));
#2319=EDGE_LOOP('',(#7547,#7548,#7549,#7550));
#2320=EDGE_LOOP('',(#7551,#7552,#7553,#7554));
#2321=EDGE_LOOP('',(#7555,#7556,#7557,#7558));
#2322=EDGE_LOOP('',(#7559,#7560,#7561,#7562));
#2323=EDGE_LOOP('',(#7563,#7564,#7565,#7566,#7567,#7568,#7569,#7570,#7571,
#7572,#7573,#7574));
#2324=EDGE_LOOP('',(#7575));
#2325=EDGE_LOOP('',(#7576,#7577,#7578,#7579));
#2326=EDGE_LOOP('',(#7580,#7581,#7582,#7583));
#2327=EDGE_LOOP('',(#7584));
#2328=EDGE_LOOP('',(#7585));
#2329=EDGE_LOOP('',(#7586,#7587,#7588,#7589));
#2330=EDGE_LOOP('',(#7590,#7591,#7592,#7593,#7594,#7595,#7596,#7597));
#2331=EDGE_LOOP('',(#7598));
#2332=EDGE_LOOP('',(#7599,#7600,#7601,#7602));
#2333=EDGE_LOOP('',(#7603,#7604,#7605,#7606));
#2334=EDGE_LOOP('',(#7607));
#2335=EDGE_LOOP('',(#7608,#7609,#7610,#7611));
#2336=EDGE_LOOP('',(#7612,#7613,#7614,#7615));
#2337=EDGE_LOOP('',(#7616));
#2338=EDGE_LOOP('',(#7617,#7618,#7619,#7620));
#2339=EDGE_LOOP('',(#7621,#7622,#7623,#7624,#7625,#7626,#7627,#7628,#7629,
#7630,#7631,#7632));
#2340=EDGE_LOOP('',(#7633));
#2341=EDGE_LOOP('',(#7634,#7635,#7636,#7637));
#2342=EDGE_LOOP('',(#7638,#7639,#7640,#7641));
#2343=EDGE_LOOP('',(#7642,#7643,#7644,#7645));
#2344=EDGE_LOOP('',(#7646,#7647,#7648,#7649));
#2345=EDGE_LOOP('',(#7650,#7651,#7652,#7653));
#2346=EDGE_LOOP('',(#7654,#7655,#7656,#7657));
#2347=EDGE_LOOP('',(#7658,#7659,#7660,#7661,#7662,#7663));
#2348=EDGE_LOOP('',(#7664,#7665,#7666,#7667,#7668,#7669));
#2349=EDGE_LOOP('',(#7670));
#2350=EDGE_LOOP('',(#7671));
#2351=EDGE_LOOP('',(#7672,#7673,#7674,#7675));
#2352=EDGE_LOOP('',(#7676,#7677,#7678,#7679));
#2353=EDGE_LOOP('',(#7680,#7681,#7682,#7683));
#2354=EDGE_LOOP('',(#7684));
#2355=EDGE_LOOP('',(#7685));
#2356=EDGE_LOOP('',(#7686,#7687,#7688,#7689));
#2357=EDGE_LOOP('',(#7690,#7691,#7692,#7693));
#2358=EDGE_LOOP('',(#7694));
#2359=EDGE_LOOP('',(#7695,#7696,#7697,#7698));
#2360=EDGE_LOOP('',(#7699,#7700,#7701,#7702));
#2361=EDGE_LOOP('',(#7703,#7704,#7705,#7706));
#2362=EDGE_LOOP('',(#7707));
#2363=EDGE_LOOP('',(#7708));
#2364=EDGE_LOOP('',(#7709,#7710,#7711,#7712));
#2365=EDGE_LOOP('',(#7713,#7714,#7715,#7716));
#2366=EDGE_LOOP('',(#7717,#7718,#7719,#7720));
#2367=EDGE_LOOP('',(#7721));
#2368=EDGE_LOOP('',(#7722,#7723,#7724,#7725));
#2369=EDGE_LOOP('',(#7726,#7727,#7728,#7729));
#2370=EDGE_LOOP('',(#7730,#7731,#7732,#7733));
#2371=EDGE_LOOP('',(#7734,#7735,#7736,#7737));
#2372=EDGE_LOOP('',(#7738,#7739,#7740,#7741));
#2373=EDGE_LOOP('',(#7742,#7743,#7744,#7745));
#2374=EDGE_LOOP('',(#7746,#7747,#7748,#7749,#7750,#7751));
#2375=EDGE_LOOP('',(#7752,#7753,#7754,#7755,#7756,#7757));
#2376=EDGE_LOOP('',(#7758,#7759,#7760,#7761));
#2377=EDGE_LOOP('',(#7762,#7763,#7764,#7765));
#2378=EDGE_LOOP('',(#7766,#7767,#7768,#7769));
#2379=EDGE_LOOP('',(#7770,#7771,#7772,#7773));
#2380=EDGE_LOOP('',(#7774,#7775,#7776,#7777));
#2381=EDGE_LOOP('',(#7778,#7779,#7780,#7781));
#2382=EDGE_LOOP('',(#7782,#7783,#7784,#7785));
#2383=EDGE_LOOP('',(#7786,#7787,#7788,#7789));
#2384=EDGE_LOOP('',(#7790,#7791,#7792,#7793));
#2385=EDGE_LOOP('',(#7794,#7795,#7796,#7797));
#2386=EDGE_LOOP('',(#7798,#7799,#7800,#7801));
#2387=EDGE_LOOP('',(#7802,#7803,#7804,#7805));
#2388=EDGE_LOOP('',(#7806,#7807,#7808,#7809));
#2389=EDGE_LOOP('',(#7810,#7811,#7812,#7813));
#2390=EDGE_LOOP('',(#7814,#7815,#7816,#7817));
#2391=EDGE_LOOP('',(#7818,#7819,#7820,#7821));
#2392=EDGE_LOOP('',(#7822,#7823,#7824,#7825));
#2393=EDGE_LOOP('',(#7826,#7827,#7828,#7829));
#2394=EDGE_LOOP('',(#7830,#7831,#7832,#7833));
#2395=EDGE_LOOP('',(#7834,#7835,#7836,#7837));
#2396=EDGE_LOOP('',(#7838,#7839,#7840,#7841));
#2397=EDGE_LOOP('',(#7842,#7843,#7844,#7845));
#2398=EDGE_LOOP('',(#7846,#7847,#7848,#7849));
#2399=EDGE_LOOP('',(#7850,#7851,#7852,#7853));
#2400=EDGE_LOOP('',(#7854,#7855,#7856,#7857));
#2401=EDGE_LOOP('',(#7858,#7859,#7860,#7861));
#2402=EDGE_LOOP('',(#7862,#7863,#7864,#7865));
#2403=EDGE_LOOP('',(#7866,#7867,#7868,#7869));
#2404=EDGE_LOOP('',(#7870,#7871,#7872,#7873));
#2405=EDGE_LOOP('',(#7874));
#2406=EDGE_LOOP('',(#7875));
#2407=EDGE_LOOP('',(#7876));
#2408=EDGE_LOOP('',(#7877));
#2409=EDGE_LOOP('',(#7878));
#2410=EDGE_LOOP('',(#7879));
#2411=EDGE_LOOP('',(#7880));
#2412=EDGE_LOOP('',(#7881));
#2413=EDGE_LOOP('',(#7882));
#2414=EDGE_LOOP('',(#7883));
#2415=EDGE_LOOP('',(#7884));
#2416=EDGE_LOOP('',(#7885));
#2417=EDGE_LOOP('',(#7886));
#2418=EDGE_LOOP('',(#7887));
#2419=EDGE_LOOP('',(#7888));
#2420=EDGE_LOOP('',(#7889));
#2421=EDGE_LOOP('',(#7890));
#2422=EDGE_LOOP('',(#7891));
#2423=EDGE_LOOP('',(#7892));
#2424=EDGE_LOOP('',(#7893));
#2425=EDGE_LOOP('',(#7894));
#2426=EDGE_LOOP('',(#7895));
#2427=EDGE_LOOP('',(#7896));
#2428=EDGE_LOOP('',(#7897));
#2429=EDGE_LOOP('',(#7898,#7899,#7900,#7901));
#2430=EDGE_LOOP('',(#7902));
#2431=EDGE_LOOP('',(#7903));
#2432=EDGE_LOOP('',(#7904));
#2433=EDGE_LOOP('',(#7905));
#2434=EDGE_LOOP('',(#7906));
#2435=EDGE_LOOP('',(#7907));
#2436=EDGE_LOOP('',(#7908));
#2437=EDGE_LOOP('',(#7909));
#2438=EDGE_LOOP('',(#7910));
#2439=EDGE_LOOP('',(#7911));
#2440=EDGE_LOOP('',(#7912));
#2441=EDGE_LOOP('',(#7913));
#2442=EDGE_LOOP('',(#7914));
#2443=EDGE_LOOP('',(#7915));
#2444=EDGE_LOOP('',(#7916));
#2445=EDGE_LOOP('',(#7917));
#2446=EDGE_LOOP('',(#7918));
#2447=EDGE_LOOP('',(#7919));
#2448=EDGE_LOOP('',(#7920));
#2449=EDGE_LOOP('',(#7921));
#2450=EDGE_LOOP('',(#7922));
#2451=EDGE_LOOP('',(#7923));
#2452=EDGE_LOOP('',(#7924));
#2453=EDGE_LOOP('',(#7925));
#2454=EDGE_LOOP('',(#7926,#7927));
#2455=EDGE_LOOP('',(#7928,#7929,#7930,#7931,#7932,#7933,#7934,#7935));
#2456=EDGE_LOOP('',(#7936,#7937));
#2457=EDGE_LOOP('',(#7938,#7939,#7940,#7941,#7942,#7943,#7944,#7945));
#2458=EDGE_LOOP('',(#7946,#7947,#7948));
#2459=EDGE_LOOP('',(#7949,#7950,#7951,#7952,#7953,#7954,#7955,#7956));
#2460=EDGE_LOOP('',(#7957,#7958,#7959));
#2461=EDGE_LOOP('',(#7960,#7961,#7962,#7963,#7964,#7965,#7966,#7967));
#2462=EDGE_LOOP('',(#7968,#7969,#7970,#7971,#7972,#7973,#7974,#7975,#7976,
#7977,#7978,#7979,#7980,#7981,#7982,#7983,#7984,#7985,#7986,#7987));
#2463=EDGE_LOOP('',(#7988,#7989,#7990,#7991));
#2464=EDGE_LOOP('',(#7992));
#2465=EDGE_LOOP('',(#7993));
#2466=EDGE_LOOP('',(#7994));
#2467=EDGE_LOOP('',(#7995,#7996,#7997,#7998,#7999,#8000,#8001,#8002,#8003,
#8004,#8005));
#2468=EDGE_LOOP('',(#8006,#8007,#8008,#8009));
#2469=EDGE_LOOP('',(#8010,#8011,#8012,#8013));
#2470=EDGE_LOOP('',(#8014));
#2471=EDGE_LOOP('',(#8015));
#2472=EDGE_LOOP('',(#8016));
#2473=EDGE_LOOP('',(#8017));
#2474=EDGE_LOOP('',(#8018));
#2475=EDGE_LOOP('',(#8019));
#2476=EDGE_LOOP('',(#8020));
#2477=EDGE_LOOP('',(#8021));
#2478=EDGE_LOOP('',(#8022,#8023));
#2479=EDGE_LOOP('',(#8024,#8025,#8026,#8027,#8028,#8029,#8030,#8031));
#2480=EDGE_LOOP('',(#8032,#8033));
#2481=EDGE_LOOP('',(#8034,#8035,#8036,#8037,#8038,#8039,#8040,#8041));
#2482=EDGE_LOOP('',(#8042,#8043,#8044));
#2483=EDGE_LOOP('',(#8045,#8046,#8047,#8048,#8049,#8050,#8051,#8052));
#2484=EDGE_LOOP('',(#8053,#8054,#8055));
#2485=EDGE_LOOP('',(#8056,#8057,#8058,#8059,#8060,#8061,#8062,#8063));
#2486=EDGE_LOOP('',(#8064,#8065,#8066,#8067,#8068,#8069,#8070,#8071,#8072,
#8073,#8074,#8075,#8076,#8077,#8078,#8079,#8080,#8081,#8082,#8083));
#2487=EDGE_LOOP('',(#8084,#8085,#8086,#8087));
#2488=EDGE_LOOP('',(#8088));
#2489=EDGE_LOOP('',(#8089));
#2490=EDGE_LOOP('',(#8090));
#2491=EDGE_LOOP('',(#8091,#8092,#8093,#8094,#8095,#8096,#8097,#8098,#8099,
#8100,#8101));
#2492=EDGE_LOOP('',(#8102,#8103,#8104,#8105));
#2493=EDGE_LOOP('',(#8106,#8107,#8108,#8109));
#2494=EDGE_LOOP('',(#8110));
#2495=EDGE_LOOP('',(#8111));
#2496=EDGE_LOOP('',(#8112));
#2497=EDGE_LOOP('',(#8113));
#2498=EDGE_LOOP('',(#8114));
#2499=EDGE_LOOP('',(#8115));
#2500=EDGE_LOOP('',(#8116));
#2501=EDGE_LOOP('',(#8117));
#2502=EDGE_LOOP('',(#8118,#8119));
#2503=EDGE_LOOP('',(#8120,#8121,#8122,#8123,#8124,#8125,#8126,#8127));
#2504=EDGE_LOOP('',(#8128,#8129));
#2505=EDGE_LOOP('',(#8130,#8131,#8132,#8133,#8134,#8135,#8136,#8137));
#2506=EDGE_LOOP('',(#8138,#8139,#8140));
#2507=EDGE_LOOP('',(#8141,#8142,#8143,#8144,#8145,#8146,#8147,#8148));
#2508=EDGE_LOOP('',(#8149,#8150,#8151));
#2509=EDGE_LOOP('',(#8152,#8153,#8154,#8155,#8156,#8157,#8158,#8159));
#2510=EDGE_LOOP('',(#8160,#8161,#8162,#8163,#8164,#8165,#8166,#8167,#8168,
#8169,#8170,#8171,#8172,#8173,#8174,#8175,#8176,#8177,#8178,#8179));
#2511=EDGE_LOOP('',(#8180,#8181,#8182,#8183));
#2512=EDGE_LOOP('',(#8184));
#2513=EDGE_LOOP('',(#8185));
#2514=EDGE_LOOP('',(#8186));
#2515=EDGE_LOOP('',(#8187,#8188,#8189,#8190,#8191,#8192,#8193,#8194,#8195,
#8196,#8197));
#2516=EDGE_LOOP('',(#8198,#8199,#8200,#8201));
#2517=EDGE_LOOP('',(#8202,#8203,#8204,#8205));
#2518=EDGE_LOOP('',(#8206));
#2519=EDGE_LOOP('',(#8207));
#2520=EDGE_LOOP('',(#8208));
#2521=EDGE_LOOP('',(#8209));
#2522=EDGE_LOOP('',(#8210));
#2523=EDGE_LOOP('',(#8211));
#2524=EDGE_LOOP('',(#8212));
#2525=EDGE_LOOP('',(#8213));
#2526=EDGE_LOOP('',(#8214,#8215));
#2527=EDGE_LOOP('',(#8216,#8217,#8218,#8219,#8220,#8221,#8222,#8223));
#2528=EDGE_LOOP('',(#8224,#8225));
#2529=EDGE_LOOP('',(#8226,#8227,#8228,#8229,#8230,#8231,#8232,#8233));
#2530=EDGE_LOOP('',(#8234,#8235,#8236));
#2531=EDGE_LOOP('',(#8237,#8238,#8239,#8240,#8241,#8242,#8243,#8244));
#2532=EDGE_LOOP('',(#8245,#8246,#8247));
#2533=EDGE_LOOP('',(#8248,#8249,#8250,#8251,#8252,#8253,#8254,#8255));
#2534=EDGE_LOOP('',(#8256,#8257,#8258,#8259,#8260,#8261,#8262,#8263,#8264,
#8265,#8266,#8267,#8268,#8269,#8270,#8271,#8272,#8273,#8274,#8275));
#2535=EDGE_LOOP('',(#8276,#8277,#8278,#8279));
#2536=EDGE_LOOP('',(#8280));
#2537=EDGE_LOOP('',(#8281));
#2538=EDGE_LOOP('',(#8282));
#2539=EDGE_LOOP('',(#8283,#8284,#8285,#8286,#8287,#8288,#8289,#8290,#8291,
#8292,#8293));
#2540=EDGE_LOOP('',(#8294,#8295,#8296,#8297));
#2541=EDGE_LOOP('',(#8298,#8299,#8300,#8301));
#2542=EDGE_LOOP('',(#8302));
#2543=EDGE_LOOP('',(#8303));
#2544=EDGE_LOOP('',(#8304));
#2545=EDGE_LOOP('',(#8305));
#2546=EDGE_LOOP('',(#8306));
#2547=EDGE_LOOP('',(#8307));
#2548=EDGE_LOOP('',(#8308));
#2549=EDGE_LOOP('',(#8309));
#2550=EDGE_LOOP('',(#8310,#8311,#8312,#8313));
#2551=EDGE_LOOP('',(#8314,#8315,#8316,#8317));
#2552=EDGE_LOOP('',(#8318,#8319,#8320,#8321));
#2553=EDGE_LOOP('',(#8322,#8323,#8324,#8325));
#2554=EDGE_LOOP('',(#8326));
#2555=EDGE_LOOP('',(#8327));
#2556=EDGE_LOOP('',(#8328));
#2557=EDGE_LOOP('',(#8329));
#2558=EDGE_LOOP('',(#8330));
#2559=EDGE_LOOP('',(#8331));
#2560=EDGE_LOOP('',(#8332,#8333,#8334,#8335));
#2561=EDGE_LOOP('',(#8336,#8337,#8338,#8339));
#2562=EDGE_LOOP('',(#8340));
#2563=EDGE_LOOP('',(#8341));
#2564=EDGE_LOOP('',(#8342));
#2565=EDGE_LOOP('',(#8343));
#2566=EDGE_LOOP('',(#8344));
#2567=EDGE_LOOP('',(#8345));
#2568=EDGE_LOOP('',(#8346,#8347,#8348,#8349));
#2569=EDGE_LOOP('',(#8350,#8351,#8352,#8353));
#2570=EDGE_LOOP('',(#8354,#8355,#8356,#8357));
#2571=EDGE_LOOP('',(#8358,#8359,#8360,#8361));
#2572=EDGE_LOOP('',(#8362,#8363,#8364,#8365));
#2573=EDGE_LOOP('',(#8366));
#2574=EDGE_LOOP('',(#8367));
#2575=EDGE_LOOP('',(#8368,#8369,#8370,#8371));
#2576=EDGE_LOOP('',(#8372));
#2577=EDGE_LOOP('',(#8373));
#2578=EDGE_LOOP('',(#8374,#8375,#8376,#8377));
#2579=EDGE_LOOP('',(#8378));
#2580=EDGE_LOOP('',(#8379));
#2581=EDGE_LOOP('',(#8380,#8381,#8382,#8383));
#2582=EDGE_LOOP('',(#8384));
#2583=EDGE_LOOP('',(#8385));
#2584=EDGE_LOOP('',(#8386,#8387,#8388,#8389));
#2585=EDGE_LOOP('',(#8390));
#2586=EDGE_LOOP('',(#8391));
#2587=EDGE_LOOP('',(#8392,#8393,#8394,#8395));
#2588=EDGE_LOOP('',(#8396));
#2589=EDGE_LOOP('',(#8397));
#2590=EDGE_LOOP('',(#8398,#8399,#8400,#8401));
#2591=EDGE_LOOP('',(#8402,#8403,#8404,#8405));
#2592=EDGE_LOOP('',(#8406,#8407,#8408,#8409));
#2593=EDGE_LOOP('',(#8410,#8411,#8412,#8413));
#2594=EDGE_LOOP('',(#8414,#8415,#8416,#8417));
#2595=EDGE_LOOP('',(#8418,#8419,#8420,#8421));
#2596=EDGE_LOOP('',(#8422));
#2597=EDGE_LOOP('',(#8423));
#2598=EDGE_LOOP('',(#8424,#8425,#8426,#8427));
#2599=EDGE_LOOP('',(#8428,#8429,#8430,#8431));
#2600=EDGE_LOOP('',(#8432));
#2601=EDGE_LOOP('',(#8433));
#2602=EDGE_LOOP('',(#8434,#8435,#8436,#8437));
#2603=EDGE_LOOP('',(#8438,#8439,#8440,#8441));
#2604=EDGE_LOOP('',(#8442));
#2605=EDGE_LOOP('',(#8443,#8444,#8445,#8446));
#2606=EDGE_LOOP('',(#8447,#8448,#8449,#8450));
#2607=EDGE_LOOP('',(#8451,#8452,#8453,#8454));
#2608=EDGE_LOOP('',(#8455));
#2609=EDGE_LOOP('',(#8456));
#2610=EDGE_LOOP('',(#8457,#8458,#8459,#8460));
#2611=EDGE_LOOP('',(#8461,#8462,#8463,#8464));
#2612=EDGE_LOOP('',(#8465,#8466,#8467,#8468));
#2613=EDGE_LOOP('',(#8469));
#2614=EDGE_LOOP('',(#8470,#8471,#8472,#8473));
#2615=EDGE_LOOP('',(#8474,#8475,#8476,#8477));
#2616=EDGE_LOOP('',(#8478,#8479,#8480,#8481));
#2617=EDGE_LOOP('',(#8482,#8483,#8484,#8485));
#2618=EDGE_LOOP('',(#8486,#8487,#8488,#8489));
#2619=EDGE_LOOP('',(#8490,#8491,#8492,#8493));
#2620=EDGE_LOOP('',(#8494,#8495,#8496,#8497,#8498,#8499));
#2621=EDGE_LOOP('',(#8500,#8501,#8502,#8503,#8504,#8505));
#2622=LINE('',#13956,#3241);
#2623=LINE('',#13962,#3242);
#2624=LINE('',#13968,#3243);
#2625=LINE('',#13974,#3244);
#2626=LINE('',#13980,#3245);
#2627=LINE('',#13986,#3246);
#2628=LINE('',#13992,#3247);
#2629=LINE('',#13998,#3248);
#2630=LINE('',#14004,#3249);
#2631=LINE('',#14010,#3250);
#2632=LINE('',#14016,#3251);
#2633=LINE('',#14022,#3252);
#2634=LINE('',#14028,#3253);
#2635=LINE('',#14034,#3254);
#2636=LINE('',#14040,#3255);
#2637=LINE('',#14046,#3256);
#2638=LINE('',#14052,#3257);
#2639=LINE('',#14058,#3258);
#2640=LINE('',#14064,#3259);
#2641=LINE('',#14070,#3260);
#2642=LINE('',#14076,#3261);
#2643=LINE('',#14082,#3262);
#2644=LINE('',#14087,#3263);
#2645=LINE('',#14089,#3264);
#2646=LINE('',#14091,#3265);
#2647=LINE('',#14092,#3266);
#2648=LINE('',#14095,#3267);
#2649=LINE('',#14097,#3268);
#2650=LINE('',#14098,#3269);
#2651=LINE('',#14101,#3270);
#2652=LINE('',#14103,#3271);
#2653=LINE('',#14104,#3272);
#2654=LINE('',#14106,#3273);
#2655=LINE('',#14107,#3274);
#2656=LINE('',#14114,#3275);
#2657=LINE('',#14116,#3276);
#2658=LINE('',#14118,#3277);
#2659=LINE('',#14119,#3278);
#2660=LINE('',#14122,#3279);
#2661=LINE('',#14124,#3280);
#2662=LINE('',#14125,#3281);
#2663=LINE('',#14128,#3282);
#2664=LINE('',#14130,#3283);
#2665=LINE('',#14131,#3284);
#2666=LINE('',#14133,#3285);
#2667=LINE('',#14134,#3286);
#2668=LINE('',#14141,#3287);
#2669=LINE('',#14143,#3288);
#2670=LINE('',#14145,#3289);
#2671=LINE('',#14146,#3290);
#2672=LINE('',#14149,#3291);
#2673=LINE('',#14151,#3292);
#2674=LINE('',#14152,#3293);
#2675=LINE('',#14155,#3294);
#2676=LINE('',#14157,#3295);
#2677=LINE('',#14158,#3296);
#2678=LINE('',#14160,#3297);
#2679=LINE('',#14161,#3298);
#2680=LINE('',#14169,#3299);
#2681=LINE('',#14175,#3300);
#2682=LINE('',#14181,#3301);
#2683=LINE('',#14187,#3302);
#2684=LINE('',#14193,#3303);
#2685=LINE('',#14199,#3304);
#2686=LINE('',#14205,#3305);
#2687=LINE('',#14211,#3306);
#2688=LINE('',#14217,#3307);
#2689=LINE('',#14223,#3308);
#2690=LINE('',#14229,#3309);
#2691=LINE('',#14235,#3310);
#2692=LINE('',#14241,#3311);
#2693=LINE('',#14247,#3312);
#2694=LINE('',#14253,#3313);
#2695=LINE('',#14259,#3314);
#2696=LINE('',#14265,#3315);
#2697=LINE('',#14271,#3316);
#2698=LINE('',#14276,#3317);
#2699=LINE('',#14278,#3318);
#2700=LINE('',#14280,#3319);
#2701=LINE('',#14281,#3320);
#2702=LINE('',#14284,#3321);
#2703=LINE('',#14286,#3322);
#2704=LINE('',#14287,#3323);
#2705=LINE('',#14290,#3324);
#2706=LINE('',#14292,#3325);
#2707=LINE('',#14293,#3326);
#2708=LINE('',#14295,#3327);
#2709=LINE('',#14296,#3328);
#2710=LINE('',#14304,#3329);
#2711=LINE('',#14311,#3330);
#2712=LINE('',#14318,#3331);
#2713=LINE('',#14325,#3332);
#2714=LINE('',#14331,#3333);
#2715=LINE('',#14333,#3334);
#2716=LINE('',#14335,#3335);
#2717=LINE('',#14336,#3336);
#2718=LINE('',#14339,#3337);
#2719=LINE('',#14341,#3338);
#2720=LINE('',#14342,#3339);
#2721=LINE('',#14345,#3340);
#2722=LINE('',#14347,#3341);
#2723=LINE('',#14348,#3342);
#2724=LINE('',#14350,#3343);
#2725=LINE('',#14351,#3344);
#2726=LINE('',#14359,#3345);
#2727=LINE('',#14366,#3346);
#2728=LINE('',#14373,#3347);
#2729=LINE('',#14380,#3348);
#2730=LINE('',#14386,#3349);
#2731=LINE('',#14388,#3350);
#2732=LINE('',#14390,#3351);
#2733=LINE('',#14391,#3352);
#2734=LINE('',#14394,#3353);
#2735=LINE('',#14396,#3354);
#2736=LINE('',#14397,#3355);
#2737=LINE('',#14400,#3356);
#2738=LINE('',#14402,#3357);
#2739=LINE('',#14403,#3358);
#2740=LINE('',#14405,#3359);
#2741=LINE('',#14406,#3360);
#2742=LINE('',#14414,#3361);
#2743=LINE('',#14421,#3362);
#2744=LINE('',#14428,#3363);
#2745=LINE('',#14434,#3364);
#2746=LINE('',#14439,#3365);
#2747=LINE('',#14441,#3366);
#2748=LINE('',#14443,#3367);
#2749=LINE('',#14444,#3368);
#2750=LINE('',#14447,#3369);
#2751=LINE('',#14449,#3370);
#2752=LINE('',#14450,#3371);
#2753=LINE('',#14453,#3372);
#2754=LINE('',#14455,#3373);
#2755=LINE('',#14456,#3374);
#2756=LINE('',#14458,#3375);
#2757=LINE('',#14459,#3376);
#2758=LINE('',#14467,#3377);
#2759=LINE('',#14473,#3378);
#2760=LINE('',#14479,#3379);
#2761=LINE('',#14483,#3380);
#2762=LINE('',#14487,#3381);
#2763=LINE('',#14490,#3382);
#2764=LINE('',#14495,#3383);
#2765=LINE('',#14499,#3384);
#2766=LINE('',#14503,#3385);
#2767=LINE('',#14506,#3386);
#2768=LINE('',#14508,#3387);
#2769=LINE('',#14510,#3388);
#2770=LINE('',#14512,#3389);
#2771=LINE('',#14514,#3390);
#2772=LINE('',#14516,#3391);
#2773=LINE('',#14517,#3392);
#2774=LINE('',#14520,#3393);
#2775=LINE('',#14522,#3394);
#2776=LINE('',#14523,#3395);
#2777=LINE('',#14527,#3396);
#2778=LINE('',#14528,#3397);
#2779=LINE('',#14529,#3398);
#2780=LINE('',#14533,#3399);
#2781=LINE('',#14534,#3400);
#2782=LINE('',#14535,#3401);
#2783=LINE('',#14539,#3402);
#2784=LINE('',#14540,#3403);
#2785=LINE('',#14541,#3404);
#2786=LINE('',#14543,#3405);
#2787=LINE('',#14544,#3406);
#2788=LINE('',#14552,#3407);
#2789=LINE('',#14558,#3408);
#2790=LINE('',#16048,#3409);
#2791=LINE('',#16055,#3410);
#2792=LINE('',#16062,#3411);
#2793=LINE('',#16068,#3412);
#2794=LINE('',#16073,#3413);
#2795=LINE('',#16075,#3414);
#2796=LINE('',#16077,#3415);
#2797=LINE('',#16078,#3416);
#2798=LINE('',#16081,#3417);
#2799=LINE('',#16083,#3418);
#2800=LINE('',#16084,#3419);
#2801=LINE('',#16087,#3420);
#2802=LINE('',#16089,#3421);
#2803=LINE('',#16090,#3422);
#2804=LINE('',#16092,#3423);
#2805=LINE('',#16093,#3424);
#2806=LINE('',#16101,#3425);
#2807=LINE('',#16107,#3426);
#2808=LINE('',#16113,#3427);
#2809=LINE('',#16117,#3428);
#2810=LINE('',#16121,#3429);
#2811=LINE('',#16124,#3430);
#2812=LINE('',#16129,#3431);
#2813=LINE('',#16133,#3432);
#2814=LINE('',#16137,#3433);
#2815=LINE('',#16140,#3434);
#2816=LINE('',#16142,#3435);
#2817=LINE('',#16144,#3436);
#2818=LINE('',#16146,#3437);
#2819=LINE('',#16148,#3438);
#2820=LINE('',#16150,#3439);
#2821=LINE('',#16151,#3440);
#2822=LINE('',#16154,#3441);
#2823=LINE('',#16156,#3442);
#2824=LINE('',#16157,#3443);
#2825=LINE('',#16161,#3444);
#2826=LINE('',#16162,#3445);
#2827=LINE('',#16163,#3446);
#2828=LINE('',#16167,#3447);
#2829=LINE('',#16168,#3448);
#2830=LINE('',#16169,#3449);
#2831=LINE('',#16173,#3450);
#2832=LINE('',#16174,#3451);
#2833=LINE('',#16175,#3452);
#2834=LINE('',#16177,#3453);
#2835=LINE('',#16178,#3454);
#2836=LINE('',#16186,#3455);
#2837=LINE('',#16192,#3456);
#2838=LINE('',#17605,#3457);
#2839=LINE('',#17612,#3458);
#2840=LINE('',#17619,#3459);
#2841=LINE('',#17625,#3460);
#2842=LINE('',#17630,#3461);
#2843=LINE('',#17632,#3462);
#2844=LINE('',#17634,#3463);
#2845=LINE('',#17635,#3464);
#2846=LINE('',#17638,#3465);
#2847=LINE('',#17640,#3466);
#2848=LINE('',#17641,#3467);
#2849=LINE('',#17644,#3468);
#2850=LINE('',#17646,#3469);
#2851=LINE('',#17647,#3470);
#2852=LINE('',#17649,#3471);
#2853=LINE('',#17650,#3472);
#2854=LINE('',#17658,#3473);
#2855=LINE('',#17664,#3474);
#2856=LINE('',#17670,#3475);
#2857=LINE('',#17674,#3476);
#2858=LINE('',#17678,#3477);
#2859=LINE('',#17681,#3478);
#2860=LINE('',#17686,#3479);
#2861=LINE('',#17690,#3480);
#2862=LINE('',#17694,#3481);
#2863=LINE('',#17697,#3482);
#2864=LINE('',#17699,#3483);
#2865=LINE('',#17701,#3484);
#2866=LINE('',#17703,#3485);
#2867=LINE('',#17705,#3486);
#2868=LINE('',#17707,#3487);
#2869=LINE('',#17708,#3488);
#2870=LINE('',#17711,#3489);
#2871=LINE('',#17713,#3490);
#2872=LINE('',#17714,#3491);
#2873=LINE('',#17718,#3492);
#2874=LINE('',#17719,#3493);
#2875=LINE('',#17720,#3494);
#2876=LINE('',#17724,#3495);
#2877=LINE('',#17725,#3496);
#2878=LINE('',#17726,#3497);
#2879=LINE('',#17730,#3498);
#2880=LINE('',#17731,#3499);
#2881=LINE('',#17732,#3500);
#2882=LINE('',#17734,#3501);
#2883=LINE('',#17735,#3502);
#2884=LINE('',#17743,#3503);
#2885=LINE('',#17749,#3504);
#2886=LINE('',#19283,#3505);
#2887=LINE('',#19290,#3506);
#2888=LINE('',#19297,#3507);
#2889=LINE('',#19303,#3508);
#2890=LINE('',#19308,#3509);
#2891=LINE('',#19310,#3510);
#2892=LINE('',#19312,#3511);
#2893=LINE('',#19313,#3512);
#2894=LINE('',#19316,#3513);
#2895=LINE('',#19318,#3514);
#2896=LINE('',#19319,#3515);
#2897=LINE('',#19322,#3516);
#2898=LINE('',#19324,#3517);
#2899=LINE('',#19325,#3518);
#2900=LINE('',#19327,#3519);
#2901=LINE('',#19328,#3520);
#2902=LINE('',#19336,#3521);
#2903=LINE('',#19342,#3522);
#2904=LINE('',#19348,#3523);
#2905=LINE('',#19352,#3524);
#2906=LINE('',#19356,#3525);
#2907=LINE('',#19359,#3526);
#2908=LINE('',#19364,#3527);
#2909=LINE('',#19368,#3528);
#2910=LINE('',#19372,#3529);
#2911=LINE('',#19375,#3530);
#2912=LINE('',#19377,#3531);
#2913=LINE('',#19379,#3532);
#2914=LINE('',#19381,#3533);
#2915=LINE('',#19383,#3534);
#2916=LINE('',#19385,#3535);
#2917=LINE('',#19386,#3536);
#2918=LINE('',#19389,#3537);
#2919=LINE('',#19391,#3538);
#2920=LINE('',#19392,#3539);
#2921=LINE('',#19396,#3540);
#2922=LINE('',#19397,#3541);
#2923=LINE('',#19398,#3542);
#2924=LINE('',#19402,#3543);
#2925=LINE('',#19403,#3544);
#2926=LINE('',#19404,#3545);
#2927=LINE('',#19408,#3546);
#2928=LINE('',#19409,#3547);
#2929=LINE('',#19410,#3548);
#2930=LINE('',#19412,#3549);
#2931=LINE('',#19413,#3550);
#2932=LINE('',#19421,#3551);
#2933=LINE('',#19427,#3552);
#2934=LINE('',#20840,#3553);
#2935=LINE('',#20847,#3554);
#2936=LINE('',#20854,#3555);
#2937=LINE('',#20861,#3556);
#2938=LINE('',#20868,#3557);
#2939=LINE('',#20875,#3558);
#2940=LINE('',#20881,#3559);
#2941=LINE('',#20883,#3560);
#2942=LINE('',#20885,#3561);
#2943=LINE('',#20886,#3562);
#2944=LINE('',#20889,#3563);
#2945=LINE('',#20891,#3564);
#2946=LINE('',#20892,#3565);
#2947=LINE('',#20895,#3566);
#2948=LINE('',#20897,#3567);
#2949=LINE('',#20898,#3568);
#2950=LINE('',#20900,#3569);
#2951=LINE('',#20901,#3570);
#2952=LINE('',#20909,#3571);
#2953=LINE('',#20915,#3572);
#2954=LINE('',#20921,#3573);
#2955=LINE('',#20927,#3574);
#2956=LINE('',#20933,#3575);
#2957=LINE('',#20939,#3576);
#2958=LINE('',#20945,#3577);
#2959=LINE('',#20951,#3578);
#2960=LINE('',#20956,#3579);
#2961=LINE('',#20958,#3580);
#2962=LINE('',#20960,#3581);
#2963=LINE('',#20961,#3582);
#2964=LINE('',#20964,#3583);
#2965=LINE('',#20966,#3584);
#2966=LINE('',#20967,#3585);
#2967=LINE('',#20970,#3586);
#2968=LINE('',#20972,#3587);
#2969=LINE('',#20973,#3588);
#2970=LINE('',#20975,#3589);
#2971=LINE('',#20976,#3590);
#2972=LINE('',#20984,#3591);
#2973=LINE('',#20990,#3592);
#2974=LINE('',#20999,#3593);
#2975=LINE('',#21006,#3594);
#2976=LINE('',#21015,#3595);
#2977=LINE('',#21024,#3596);
#2978=LINE('',#21031,#3597);
#2979=LINE('',#21040,#3598);
#2980=LINE('',#21049,#3599);
#2981=LINE('',#21056,#3600);
#2982=LINE('',#21065,#3601);
#2983=LINE('',#21074,#3602);
#2984=LINE('',#21081,#3603);
#2985=LINE('',#21090,#3604);
#2986=LINE('',#21099,#3605);
#2987=LINE('',#21104,#3606);
#2988=LINE('',#21109,#3607);
#2989=LINE('',#21115,#3608);
#2990=LINE('',#21119,#3609);
#2991=LINE('',#21122,#3610);
#2992=LINE('',#21126,#3611);
#2993=LINE('',#21130,#3612);
#2994=LINE('',#21133,#3613);
#2995=LINE('',#21136,#3614);
#2996=LINE('',#21138,#3615);
#2997=LINE('',#21140,#3616);
#2998=LINE('',#21142,#3617);
#2999=LINE('',#21143,#3618);
#3000=LINE('',#21148,#3619);
#3001=LINE('',#21150,#3620);
#3002=LINE('',#21151,#3621);
#3003=LINE('',#21157,#3622);
#3004=LINE('',#21159,#3623);
#3005=LINE('',#21160,#3624);
#3006=LINE('',#21162,#3625);
#3007=LINE('',#21163,#3626);
#3008=LINE('',#21170,#3627);
#3009=LINE('',#21174,#3628);
#3010=LINE('',#21179,#3629);
#3011=LINE('',#21183,#3630);
#3012=LINE('',#21188,#3631);
#3013=LINE('',#21192,#3632);
#3014=LINE('',#21194,#3633);
#3015=LINE('',#21195,#3634);
#3016=LINE('',#21197,#3635);
#3017=LINE('',#21199,#3636);
#3018=LINE('',#21201,#3637);
#3019=LINE('',#21203,#3638);
#3020=LINE('',#21205,#3639);
#3021=LINE('',#21206,#3640);
#3022=LINE('',#21209,#3641);
#3023=LINE('',#21210,#3642);
#3024=LINE('',#21213,#3643);
#3025=LINE('',#21214,#3644);
#3026=LINE('',#21216,#3645);
#3027=LINE('',#21219,#3646);
#3028=LINE('',#21220,#3647);
#3029=LINE('',#21223,#3648);
#3030=LINE('',#21224,#3649);
#3031=LINE('',#21227,#3650);
#3032=LINE('',#21228,#3651);
#3033=LINE('',#21231,#3652);
#3034=LINE('',#21232,#3653);
#3035=LINE('',#21235,#3654);
#3036=LINE('',#21236,#3655);
#3037=LINE('',#21238,#3656);
#3038=LINE('',#21244,#3657);
#3039=LINE('',#21246,#3658);
#3040=LINE('',#21248,#3659);
#3041=LINE('',#21249,#3660);
#3042=LINE('',#21252,#3661);
#3043=LINE('',#21254,#3662);
#3044=LINE('',#21255,#3663);
#3045=LINE('',#21258,#3664);
#3046=LINE('',#21260,#3665);
#3047=LINE('',#21261,#3666);
#3048=LINE('',#21264,#3667);
#3049=LINE('',#21266,#3668);
#3050=LINE('',#21267,#3669);
#3051=LINE('',#21270,#3670);
#3052=LINE('',#21272,#3671);
#3053=LINE('',#21273,#3672);
#3054=LINE('',#21275,#3673);
#3055=LINE('',#21276,#3674);
#3056=LINE('',#21288,#3675);
#3057=LINE('',#21292,#3676);
#3058=LINE('',#21296,#3677);
#3059=LINE('',#21303,#3678);
#3060=LINE('',#21305,#3679);
#3061=LINE('',#21313,#3680);
#3062=LINE('',#21317,#3681);
#3063=LINE('',#21321,#3682);
#3064=LINE('',#21328,#3683);
#3065=LINE('',#21332,#3684);
#3066=LINE('',#21336,#3685);
#3067=LINE('',#21341,#3686);
#3068=LINE('',#21343,#3687);
#3069=LINE('',#21345,#3688);
#3070=LINE('',#21346,#3689);
#3071=LINE('',#21349,#3690);
#3072=LINE('',#21351,#3691);
#3073=LINE('',#21352,#3692);
#3074=LINE('',#21355,#3693);
#3075=LINE('',#21357,#3694);
#3076=LINE('',#21358,#3695);
#3077=LINE('',#21361,#3696);
#3078=LINE('',#21363,#3697);
#3079=LINE('',#21364,#3698);
#3080=LINE('',#21367,#3699);
#3081=LINE('',#21369,#3700);
#3082=LINE('',#21370,#3701);
#3083=LINE('',#21372,#3702);
#3084=LINE('',#21373,#3703);
#3085=LINE('',#21382,#3704);
#3086=LINE('',#21388,#3705);
#3087=LINE('',#21394,#3706);
#3088=LINE('',#21400,#3707);
#3089=LINE('',#21406,#3708);
#3090=LINE('',#21412,#3709);
#3091=LINE('',#21418,#3710);
#3092=LINE('',#21424,#3711);
#3093=LINE('',#21430,#3712);
#3094=LINE('',#21436,#3713);
#3095=LINE('',#21442,#3714);
#3096=LINE('',#21448,#3715);
#3097=LINE('',#21454,#3716);
#3098=LINE('',#21460,#3717);
#3099=LINE('',#21466,#3718);
#3100=LINE('',#21472,#3719);
#3101=LINE('',#21478,#3720);
#3102=LINE('',#21484,#3721);
#3103=LINE('',#21490,#3722);
#3104=LINE('',#21496,#3723);
#3105=LINE('',#21502,#3724);
#3106=LINE('',#21508,#3725);
#3107=LINE('',#21514,#3726);
#3108=LINE('',#21520,#3727);
#3109=LINE('',#21525,#3728);
#3110=LINE('',#21527,#3729);
#3111=LINE('',#21529,#3730);
#3112=LINE('',#21530,#3731);
#3113=LINE('',#21533,#3732);
#3114=LINE('',#21535,#3733);
#3115=LINE('',#21536,#3734);
#3116=LINE('',#21539,#3735);
#3117=LINE('',#21541,#3736);
#3118=LINE('',#21542,#3737);
#3119=LINE('',#21544,#3738);
#3120=LINE('',#21545,#3739);
#3121=LINE('',#21556,#3740);
#3122=LINE('',#21560,#3741);
#3123=LINE('',#21564,#3742);
#3124=LINE('',#21572,#3743);
#3125=LINE('',#21576,#3744);
#3126=LINE('',#21580,#3745);
#3127=LINE('',#21590,#3746);
#3128=LINE('',#21593,#3747);
#3129=LINE('',#21595,#3748);
#3130=LINE('',#21606,#3749);
#3131=LINE('',#21609,#3750);
#3132=LINE('',#21611,#3751);
#3133=LINE('',#21617,#3752);
#3134=LINE('',#21627,#3753);
#3135=LINE('',#21638,#3754);
#3136=LINE('',#21641,#3755);
#3137=LINE('',#21653,#3756);
#3138=LINE('',#21657,#3757);
#3139=LINE('',#21661,#3758);
#3140=LINE('',#21669,#3759);
#3141=LINE('',#21673,#3760);
#3142=LINE('',#21677,#3761);
#3143=LINE('',#21687,#3762);
#3144=LINE('',#21690,#3763);
#3145=LINE('',#21692,#3764);
#3146=LINE('',#21703,#3765);
#3147=LINE('',#21706,#3766);
#3148=LINE('',#21708,#3767);
#3149=LINE('',#21714,#3768);
#3150=LINE('',#21724,#3769);
#3151=LINE('',#21735,#3770);
#3152=LINE('',#21738,#3771);
#3153=LINE('',#21750,#3772);
#3154=LINE('',#21754,#3773);
#3155=LINE('',#21758,#3774);
#3156=LINE('',#21766,#3775);
#3157=LINE('',#21770,#3776);
#3158=LINE('',#21774,#3777);
#3159=LINE('',#21784,#3778);
#3160=LINE('',#21787,#3779);
#3161=LINE('',#21789,#3780);
#3162=LINE('',#21800,#3781);
#3163=LINE('',#21803,#3782);
#3164=LINE('',#21805,#3783);
#3165=LINE('',#21811,#3784);
#3166=LINE('',#21821,#3785);
#3167=LINE('',#21832,#3786);
#3168=LINE('',#21835,#3787);
#3169=LINE('',#21847,#3788);
#3170=LINE('',#21851,#3789);
#3171=LINE('',#21855,#3790);
#3172=LINE('',#21863,#3791);
#3173=LINE('',#21867,#3792);
#3174=LINE('',#21871,#3793);
#3175=LINE('',#21881,#3794);
#3176=LINE('',#21884,#3795);
#3177=LINE('',#21886,#3796);
#3178=LINE('',#21897,#3797);
#3179=LINE('',#21900,#3798);
#3180=LINE('',#21902,#3799);
#3181=LINE('',#21908,#3800);
#3182=LINE('',#21918,#3801);
#3183=LINE('',#21929,#3802);
#3184=LINE('',#21932,#3803);
#3185=LINE('',#21941,#3804);
#3186=LINE('',#21947,#3805);
#3187=LINE('',#21953,#3806);
#3188=LINE('',#21959,#3807);
#3189=LINE('',#21969,#3808);
#3190=LINE('',#21972,#3809);
#3191=LINE('',#21983,#3810);
#3192=LINE('',#21985,#3811);
#3193=LINE('',#21986,#3812);
#3194=LINE('',#21989,#3813);
#3195=LINE('',#21991,#3814);
#3196=LINE('',#21992,#3815);
#3197=LINE('',#21997,#3816);
#3198=LINE('',#21998,#3817);
#3199=LINE('',#22000,#3818);
#3200=LINE('',#22001,#3819);
#3201=LINE('',#22011,#3820);
#3202=LINE('',#22018,#3821);
#3203=LINE('',#22025,#3822);
#3204=LINE('',#22032,#3823);
#3205=LINE('',#22039,#3824);
#3206=LINE('',#22044,#3825);
#3207=LINE('',#22051,#3826);
#3208=LINE('',#22054,#3827);
#3209=LINE('',#22057,#3828);
#3210=LINE('',#22059,#3829);
#3211=LINE('',#22060,#3830);
#3212=LINE('',#22066,#3831);
#3213=LINE('',#22068,#3832);
#3214=LINE('',#22069,#3833);
#3215=LINE('',#22078,#3834);
#3216=LINE('',#22083,#3835);
#3217=LINE('',#22093,#3836);
#3218=LINE('',#22097,#3837);
#3219=LINE('',#22101,#3838);
#3220=LINE('',#22108,#3839);
#3221=LINE('',#22112,#3840);
#3222=LINE('',#22116,#3841);
#3223=LINE('',#22121,#3842);
#3224=LINE('',#22123,#3843);
#3225=LINE('',#22125,#3844);
#3226=LINE('',#22126,#3845);
#3227=LINE('',#22129,#3846);
#3228=LINE('',#22131,#3847);
#3229=LINE('',#22132,#3848);
#3230=LINE('',#22135,#3849);
#3231=LINE('',#22137,#3850);
#3232=LINE('',#22138,#3851);
#3233=LINE('',#22141,#3852);
#3234=LINE('',#22143,#3853);
#3235=LINE('',#22144,#3854);
#3236=LINE('',#22147,#3855);
#3237=LINE('',#22149,#3856);
#3238=LINE('',#22150,#3857);
#3239=LINE('',#22152,#3858);
#3240=LINE('',#22153,#3859);
#3241=VECTOR('',#10960,0.275);
#3242=VECTOR('',#10967,0.275);
#3243=VECTOR('',#10974,0.5);
#3244=VECTOR('',#10981,0.5);
#3245=VECTOR('',#10988,0.5);
#3246=VECTOR('',#10995,0.5);
#3247=VECTOR('',#11002,0.21);
#3248=VECTOR('',#11009,0.21);
#3249=VECTOR('',#11016,0.21);
#3250=VECTOR('',#11023,0.21);
#3251=VECTOR('',#11030,0.275);
#3252=VECTOR('',#11037,0.275);
#3253=VECTOR('',#11044,0.275);
#3254=VECTOR('',#11051,0.275);
#3255=VECTOR('',#11058,0.275);
#3256=VECTOR('',#11065,0.275);
#3257=VECTOR('',#11072,0.275);
#3258=VECTOR('',#11079,0.275);
#3259=VECTOR('',#11086,0.275);
#3260=VECTOR('',#11093,0.275);
#3261=VECTOR('',#11100,0.275);
#3262=VECTOR('',#11107,0.275);
#3263=VECTOR('',#11112,1.);
#3264=VECTOR('',#11113,1.);
#3265=VECTOR('',#11114,1.);
#3266=VECTOR('',#11115,1.);
#3267=VECTOR('',#11118,1.);
#3268=VECTOR('',#11119,1.);
#3269=VECTOR('',#11120,1.);
#3270=VECTOR('',#11123,1.);
#3271=VECTOR('',#11124,1.);
#3272=VECTOR('',#11125,1.);
#3273=VECTOR('',#11128,1.);
#3274=VECTOR('',#11129,1.);
#3275=VECTOR('',#11138,1.);
#3276=VECTOR('',#11139,1.);
#3277=VECTOR('',#11140,1.);
#3278=VECTOR('',#11141,1.);
#3279=VECTOR('',#11144,1.);
#3280=VECTOR('',#11145,1.);
#3281=VECTOR('',#11146,1.);
#3282=VECTOR('',#11149,1.);
#3283=VECTOR('',#11150,1.);
#3284=VECTOR('',#11151,1.);
#3285=VECTOR('',#11154,1.);
#3286=VECTOR('',#11155,1.);
#3287=VECTOR('',#11164,1.);
#3288=VECTOR('',#11165,1.);
#3289=VECTOR('',#11166,1.);
#3290=VECTOR('',#11167,1.);
#3291=VECTOR('',#11170,1.);
#3292=VECTOR('',#11171,1.);
#3293=VECTOR('',#11172,1.);
#3294=VECTOR('',#11175,1.);
#3295=VECTOR('',#11176,1.);
#3296=VECTOR('',#11177,1.);
#3297=VECTOR('',#11180,1.);
#3298=VECTOR('',#11181,1.);
#3299=VECTOR('',#11192,0.275);
#3300=VECTOR('',#11199,0.275);
#3301=VECTOR('',#11206,0.275);
#3302=VECTOR('',#11213,0.275);
#3303=VECTOR('',#11220,0.275);
#3304=VECTOR('',#11227,0.275);
#3305=VECTOR('',#11234,0.275);
#3306=VECTOR('',#11241,0.275);
#3307=VECTOR('',#11248,0.275);
#3308=VECTOR('',#11255,0.275);
#3309=VECTOR('',#11262,0.275);
#3310=VECTOR('',#11269,0.275);
#3311=VECTOR('',#11276,0.275);
#3312=VECTOR('',#11283,0.275);
#3313=VECTOR('',#11290,0.61);
#3314=VECTOR('',#11297,0.61);
#3315=VECTOR('',#11304,0.61);
#3316=VECTOR('',#11311,0.61);
#3317=VECTOR('',#11316,1.);
#3318=VECTOR('',#11317,1.);
#3319=VECTOR('',#11318,1.);
#3320=VECTOR('',#11319,1.);
#3321=VECTOR('',#11322,1.);
#3322=VECTOR('',#11323,1.);
#3323=VECTOR('',#11324,1.);
#3324=VECTOR('',#11327,1.);
#3325=VECTOR('',#11328,1.);
#3326=VECTOR('',#11329,1.);
#3327=VECTOR('',#11332,1.);
#3328=VECTOR('',#11333,1.);
#3329=VECTOR('',#11344,0.210000000000001);
#3330=VECTOR('',#11353,0.210000000000001);
#3331=VECTOR('',#11362,0.210000000000001);
#3332=VECTOR('',#11371,0.210000000000001);
#3333=VECTOR('',#11378,1.);
#3334=VECTOR('',#11379,1.);
#3335=VECTOR('',#11380,1.);
#3336=VECTOR('',#11381,1.);
#3337=VECTOR('',#11384,1.);
#3338=VECTOR('',#11385,1.);
#3339=VECTOR('',#11386,1.);
#3340=VECTOR('',#11389,1.);
#3341=VECTOR('',#11390,1.);
#3342=VECTOR('',#11391,1.);
#3343=VECTOR('',#11394,1.);
#3344=VECTOR('',#11395,1.);
#3345=VECTOR('',#11406,0.210000000000001);
#3346=VECTOR('',#11415,0.210000000000001);
#3347=VECTOR('',#11424,0.210000000000001);
#3348=VECTOR('',#11433,0.210000000000001);
#3349=VECTOR('',#11440,1.);
#3350=VECTOR('',#11441,1.);
#3351=VECTOR('',#11442,1.);
#3352=VECTOR('',#11443,1.);
#3353=VECTOR('',#11446,1.);
#3354=VECTOR('',#11447,1.);
#3355=VECTOR('',#11448,1.);
#3356=VECTOR('',#11451,1.);
#3357=VECTOR('',#11452,1.);
#3358=VECTOR('',#11453,1.);
#3359=VECTOR('',#11456,1.);
#3360=VECTOR('',#11457,1.);
#3361=VECTOR('',#11468,0.21);
#3362=VECTOR('',#11477,0.21);
#3363=VECTOR('',#11486,0.21);
#3364=VECTOR('',#11493,0.21);
#3365=VECTOR('',#11498,1.);
#3366=VECTOR('',#11499,1.);
#3367=VECTOR('',#11500,1.);
#3368=VECTOR('',#11501,1.);
#3369=VECTOR('',#11504,1.);
#3370=VECTOR('',#11505,1.);
#3371=VECTOR('',#11506,1.);
#3372=VECTOR('',#11509,1.);
#3373=VECTOR('',#11510,1.);
#3374=VECTOR('',#11511,1.);
#3375=VECTOR('',#11514,1.);
#3376=VECTOR('',#11515,1.);
#3377=VECTOR('',#11526,0.21);
#3378=VECTOR('',#11533,0.21);
#3379=VECTOR('',#11540,0.21);
#3380=VECTOR('',#11543,1.);
#3381=VECTOR('',#11546,1.);
#3382=VECTOR('',#11551,1.);
#3383=VECTOR('',#11556,0.21);
#3384=VECTOR('',#11559,1.);
#3385=VECTOR('',#11562,1.);
#3386=VECTOR('',#11567,1.);
#3387=VECTOR('',#11570,1.);
#3388=VECTOR('',#11571,1.);
#3389=VECTOR('',#11572,1.);
#3390=VECTOR('',#11573,1.);
#3391=VECTOR('',#11574,1.);
#3392=VECTOR('',#11575,1.);
#3393=VECTOR('',#11578,1.);
#3394=VECTOR('',#11579,1.);
#3395=VECTOR('',#11580,1.);
#3396=VECTOR('',#11583,1.);
#3397=VECTOR('',#11584,1.);
#3398=VECTOR('',#11585,1.);
#3399=VECTOR('',#11588,1.);
#3400=VECTOR('',#11589,1.);
#3401=VECTOR('',#11590,1.);
#3402=VECTOR('',#11593,1.);
#3403=VECTOR('',#11594,1.);
#3404=VECTOR('',#11595,1.);
#3405=VECTOR('',#11598,1.);
#3406=VECTOR('',#11599,1.);
#3407=VECTOR('',#11610,0.625);
#3408=VECTOR('',#11617,1.5);
#3409=VECTOR('',#11640,0.21);
#3410=VECTOR('',#11649,0.21);
#3411=VECTOR('',#11658,0.21);
#3412=VECTOR('',#11665,0.21);
#3413=VECTOR('',#11670,1.);
#3414=VECTOR('',#11671,1.);
#3415=VECTOR('',#11672,1.);
#3416=VECTOR('',#11673,1.);
#3417=VECTOR('',#11676,1.);
#3418=VECTOR('',#11677,1.);
#3419=VECTOR('',#11678,1.);
#3420=VECTOR('',#11681,1.);
#3421=VECTOR('',#11682,1.);
#3422=VECTOR('',#11683,1.);
#3423=VECTOR('',#11686,1.);
#3424=VECTOR('',#11687,1.);
#3425=VECTOR('',#11698,0.21);
#3426=VECTOR('',#11705,0.21);
#3427=VECTOR('',#11712,0.21);
#3428=VECTOR('',#11715,1.);
#3429=VECTOR('',#11718,1.);
#3430=VECTOR('',#11723,1.);
#3431=VECTOR('',#11728,0.21);
#3432=VECTOR('',#11731,1.);
#3433=VECTOR('',#11734,1.);
#3434=VECTOR('',#11739,1.);
#3435=VECTOR('',#11742,1.);
#3436=VECTOR('',#11743,1.);
#3437=VECTOR('',#11744,1.);
#3438=VECTOR('',#11745,1.);
#3439=VECTOR('',#11746,1.);
#3440=VECTOR('',#11747,1.);
#3441=VECTOR('',#11750,1.);
#3442=VECTOR('',#11751,1.);
#3443=VECTOR('',#11752,1.);
#3444=VECTOR('',#11755,1.);
#3445=VECTOR('',#11756,1.);
#3446=VECTOR('',#11757,1.);
#3447=VECTOR('',#11760,1.);
#3448=VECTOR('',#11761,1.);
#3449=VECTOR('',#11762,1.);
#3450=VECTOR('',#11765,1.);
#3451=VECTOR('',#11766,1.);
#3452=VECTOR('',#11767,1.);
#3453=VECTOR('',#11770,1.);
#3454=VECTOR('',#11771,1.);
#3455=VECTOR('',#11782,0.625);
#3456=VECTOR('',#11789,1.5);
#3457=VECTOR('',#11812,0.21);
#3458=VECTOR('',#11821,0.21);
#3459=VECTOR('',#11830,0.21);
#3460=VECTOR('',#11837,0.21);
#3461=VECTOR('',#11842,1.);
#3462=VECTOR('',#11843,1.);
#3463=VECTOR('',#11844,1.);
#3464=VECTOR('',#11845,1.);
#3465=VECTOR('',#11848,1.);
#3466=VECTOR('',#11849,1.);
#3467=VECTOR('',#11850,1.);
#3468=VECTOR('',#11853,1.);
#3469=VECTOR('',#11854,1.);
#3470=VECTOR('',#11855,1.);
#3471=VECTOR('',#11858,1.);
#3472=VECTOR('',#11859,1.);
#3473=VECTOR('',#11870,0.21);
#3474=VECTOR('',#11877,0.21);
#3475=VECTOR('',#11884,0.21);
#3476=VECTOR('',#11887,1.);
#3477=VECTOR('',#11890,1.);
#3478=VECTOR('',#11895,1.);
#3479=VECTOR('',#11900,0.21);
#3480=VECTOR('',#11903,1.);
#3481=VECTOR('',#11906,1.);
#3482=VECTOR('',#11911,1.);
#3483=VECTOR('',#11914,1.);
#3484=VECTOR('',#11915,1.);
#3485=VECTOR('',#11916,1.);
#3486=VECTOR('',#11917,1.);
#3487=VECTOR('',#11918,1.);
#3488=VECTOR('',#11919,1.);
#3489=VECTOR('',#11922,1.);
#3490=VECTOR('',#11923,1.);
#3491=VECTOR('',#11924,1.);
#3492=VECTOR('',#11927,1.);
#3493=VECTOR('',#11928,1.);
#3494=VECTOR('',#11929,1.);
#3495=VECTOR('',#11932,1.);
#3496=VECTOR('',#11933,1.);
#3497=VECTOR('',#11934,1.);
#3498=VECTOR('',#11937,1.);
#3499=VECTOR('',#11938,1.);
#3500=VECTOR('',#11939,1.);
#3501=VECTOR('',#11942,1.);
#3502=VECTOR('',#11943,1.);
#3503=VECTOR('',#11954,0.625);
#3504=VECTOR('',#11961,1.5);
#3505=VECTOR('',#11984,0.21);
#3506=VECTOR('',#11993,0.21);
#3507=VECTOR('',#12002,0.21);
#3508=VECTOR('',#12009,0.21);
#3509=VECTOR('',#12014,1.);
#3510=VECTOR('',#12015,1.);
#3511=VECTOR('',#12016,1.);
#3512=VECTOR('',#12017,1.);
#3513=VECTOR('',#12020,1.);
#3514=VECTOR('',#12021,1.);
#3515=VECTOR('',#12022,1.);
#3516=VECTOR('',#12025,1.);
#3517=VECTOR('',#12026,1.);
#3518=VECTOR('',#12027,1.);
#3519=VECTOR('',#12030,1.);
#3520=VECTOR('',#12031,1.);
#3521=VECTOR('',#12042,0.21);
#3522=VECTOR('',#12049,0.21);
#3523=VECTOR('',#12056,0.21);
#3524=VECTOR('',#12059,1.);
#3525=VECTOR('',#12062,1.);
#3526=VECTOR('',#12067,1.);
#3527=VECTOR('',#12072,0.21);
#3528=VECTOR('',#12075,1.);
#3529=VECTOR('',#12078,1.);
#3530=VECTOR('',#12083,1.);
#3531=VECTOR('',#12086,1.);
#3532=VECTOR('',#12087,1.);
#3533=VECTOR('',#12088,1.);
#3534=VECTOR('',#12089,1.);
#3535=VECTOR('',#12090,1.);
#3536=VECTOR('',#12091,1.);
#3537=VECTOR('',#12094,1.);
#3538=VECTOR('',#12095,1.);
#3539=VECTOR('',#12096,1.);
#3540=VECTOR('',#12099,1.);
#3541=VECTOR('',#12100,1.);
#3542=VECTOR('',#12101,1.);
#3543=VECTOR('',#12104,1.);
#3544=VECTOR('',#12105,1.);
#3545=VECTOR('',#12106,1.);
#3546=VECTOR('',#12109,1.);
#3547=VECTOR('',#12110,1.);
#3548=VECTOR('',#12111,1.);
#3549=VECTOR('',#12114,1.);
#3550=VECTOR('',#12115,1.);
#3551=VECTOR('',#12126,0.625);
#3552=VECTOR('',#12133,1.5);
#3553=VECTOR('',#12156,0.21);
#3554=VECTOR('',#12165,0.21);
#3555=VECTOR('',#12174,0.21);
#3556=VECTOR('',#12183,0.21);
#3557=VECTOR('',#12192,0.6);
#3558=VECTOR('',#12201,0.8);
#3559=VECTOR('',#12208,1.);
#3560=VECTOR('',#12209,1.);
#3561=VECTOR('',#12210,1.);
#3562=VECTOR('',#12211,1.);
#3563=VECTOR('',#12214,1.);
#3564=VECTOR('',#12215,1.);
#3565=VECTOR('',#12216,1.);
#3566=VECTOR('',#12219,1.);
#3567=VECTOR('',#12220,1.);
#3568=VECTOR('',#12221,1.);
#3569=VECTOR('',#12224,1.);
#3570=VECTOR('',#12225,1.);
#3571=VECTOR('',#12236,0.275);
#3572=VECTOR('',#12243,0.275);
#3573=VECTOR('',#12250,0.275);
#3574=VECTOR('',#12257,0.275);
#3575=VECTOR('',#12264,0.275);
#3576=VECTOR('',#12271,0.275);
#3577=VECTOR('',#12278,0.275);
#3578=VECTOR('',#12285,0.275);
#3579=VECTOR('',#12290,1.);
#3580=VECTOR('',#12291,1.);
#3581=VECTOR('',#12292,1.);
#3582=VECTOR('',#12293,1.);
#3583=VECTOR('',#12296,1.);
#3584=VECTOR('',#12297,1.);
#3585=VECTOR('',#12298,1.);
#3586=VECTOR('',#12301,1.);
#3587=VECTOR('',#12302,1.);
#3588=VECTOR('',#12303,1.);
#3589=VECTOR('',#12306,1.);
#3590=VECTOR('',#12307,1.);
#3591=VECTOR('',#12318,0.51);
#3592=VECTOR('',#12325,0.8);
#3593=VECTOR('',#12338,0.21);
#3594=VECTOR('',#12347,0.5);
#3595=VECTOR('',#12360,0.5);
#3596=VECTOR('',#12373,0.21);
#3597=VECTOR('',#12382,0.5);
#3598=VECTOR('',#12395,0.5);
#3599=VECTOR('',#12408,0.21);
#3600=VECTOR('',#12417,0.5);
#3601=VECTOR('',#12430,0.5);
#3602=VECTOR('',#12443,0.21);
#3603=VECTOR('',#12452,0.5);
#3604=VECTOR('',#12465,0.5);
#3605=VECTOR('',#12478,0.55);
#3606=VECTOR('',#12485,0.6);
#3607=VECTOR('',#12492,0.55);
#3608=VECTOR('',#12499,1.);
#3609=VECTOR('',#12504,1.);
#3610=VECTOR('',#12507,1.);
#3611=VECTOR('',#12510,1.);
#3612=VECTOR('',#12513,1.);
#3613=VECTOR('',#12518,1.);
#3614=VECTOR('',#12521,1.);
#3615=VECTOR('',#12522,1.);
#3616=VECTOR('',#12523,1.);
#3617=VECTOR('',#12524,1.);
#3618=VECTOR('',#12525,1.);
#3619=VECTOR('',#12530,1.);
#3620=VECTOR('',#12531,1.);
#3621=VECTOR('',#12532,1.);
#3622=VECTOR('',#12537,1.);
#3623=VECTOR('',#12538,1.);
#3624=VECTOR('',#12539,1.);
#3625=VECTOR('',#12540,1.);
#3626=VECTOR('',#12541,1.);
#3627=VECTOR('',#12548,0.225);
#3628=VECTOR('',#12553,0.165);
#3629=VECTOR('',#12560,0.275);
#3630=VECTOR('',#12565,0.275);
#3631=VECTOR('',#12570,0.6);
#3632=VECTOR('',#12575,1.);
#3633=VECTOR('',#12576,1.);
#3634=VECTOR('',#12577,1.);
#3635=VECTOR('',#12578,1.);
#3636=VECTOR('',#12579,1.);
#3637=VECTOR('',#12580,1.);
#3638=VECTOR('',#12581,1.);
#3639=VECTOR('',#12582,1.);
#3640=VECTOR('',#12583,1.);
#3641=VECTOR('',#12586,1.);
#3642=VECTOR('',#12587,1.);
#3643=VECTOR('',#12590,1.);
#3644=VECTOR('',#12591,1.);
#3645=VECTOR('',#12594,1.);
#3646=VECTOR('',#12597,1.);
#3647=VECTOR('',#12598,1.);
#3648=VECTOR('',#12601,1.);
#3649=VECTOR('',#12602,1.);
#3650=VECTOR('',#12605,1.);
#3651=VECTOR('',#12606,1.);
#3652=VECTOR('',#12609,1.);
#3653=VECTOR('',#12610,1.);
#3654=VECTOR('',#12613,1.);
#3655=VECTOR('',#12614,1.);
#3656=VECTOR('',#12617,1.);
#3657=VECTOR('',#12624,1.);
#3658=VECTOR('',#12625,1.);
#3659=VECTOR('',#12626,1.);
#3660=VECTOR('',#12627,1.);
#3661=VECTOR('',#12630,1.);
#3662=VECTOR('',#12631,1.);
#3663=VECTOR('',#12632,1.);
#3664=VECTOR('',#12635,1.);
#3665=VECTOR('',#12636,1.);
#3666=VECTOR('',#12637,1.);
#3667=VECTOR('',#12640,1.);
#3668=VECTOR('',#12641,1.);
#3669=VECTOR('',#12642,1.);
#3670=VECTOR('',#12645,1.);
#3671=VECTOR('',#12646,1.);
#3672=VECTOR('',#12647,1.);
#3673=VECTOR('',#12650,1.);
#3674=VECTOR('',#12651,1.);
#3675=VECTOR('',#12668,0.4);
#3676=VECTOR('',#12673,0.425);
#3677=VECTOR('',#12678,0.41);
#3678=VECTOR('',#12687,0.26);
#3679=VECTOR('',#12690,0.25);
#3680=VECTOR('',#12701,0.4);
#3681=VECTOR('',#12706,0.425);
#3682=VECTOR('',#12711,0.41);
#3683=VECTOR('',#12720,0.26);
#3684=VECTOR('',#12725,0.25);
#3685=VECTOR('',#12730,0.225);
#3686=VECTOR('',#12735,1.);
#3687=VECTOR('',#12736,1.);
#3688=VECTOR('',#12737,1.);
#3689=VECTOR('',#12738,1.);
#3690=VECTOR('',#12741,1.);
#3691=VECTOR('',#12742,1.);
#3692=VECTOR('',#12743,1.);
#3693=VECTOR('',#12746,1.);
#3694=VECTOR('',#12747,1.);
#3695=VECTOR('',#12748,1.);
#3696=VECTOR('',#12751,1.);
#3697=VECTOR('',#12752,1.);
#3698=VECTOR('',#12753,1.);
#3699=VECTOR('',#12756,1.);
#3700=VECTOR('',#12757,1.);
#3701=VECTOR('',#12758,1.);
#3702=VECTOR('',#12761,1.);
#3703=VECTOR('',#12762,1.);
#3704=VECTOR('',#12775,0.225);
#3705=VECTOR('',#12782,0.225);
#3706=VECTOR('',#12789,0.225);
#3707=VECTOR('',#12796,0.225);
#3708=VECTOR('',#12803,0.225);
#3709=VECTOR('',#12810,0.225);
#3710=VECTOR('',#12817,0.225);
#3711=VECTOR('',#12824,0.225);
#3712=VECTOR('',#12831,0.225);
#3713=VECTOR('',#12838,0.225);
#3714=VECTOR('',#12845,0.225);
#3715=VECTOR('',#12852,0.225);
#3716=VECTOR('',#12859,0.225);
#3717=VECTOR('',#12866,0.225);
#3718=VECTOR('',#12873,0.225);
#3719=VECTOR('',#12880,0.225);
#3720=VECTOR('',#12887,0.225);
#3721=VECTOR('',#12894,0.225);
#3722=VECTOR('',#12901,0.225);
#3723=VECTOR('',#12908,0.225);
#3724=VECTOR('',#12915,0.625);
#3725=VECTOR('',#12922,0.625);
#3726=VECTOR('',#12929,0.625);
#3727=VECTOR('',#12936,0.625);
#3728=VECTOR('',#12941,1.);
#3729=VECTOR('',#12942,1.);
#3730=VECTOR('',#12943,1.);
#3731=VECTOR('',#12944,1.);
#3732=VECTOR('',#12947,1.);
#3733=VECTOR('',#12948,1.);
#3734=VECTOR('',#12949,1.);
#3735=VECTOR('',#12952,1.);
#3736=VECTOR('',#12953,1.);
#3737=VECTOR('',#12954,1.);
#3738=VECTOR('',#12957,1.);
#3739=VECTOR('',#12958,1.);
#3740=VECTOR('',#12973,1.);
#3741=VECTOR('',#12976,0.165);
#3742=VECTOR('',#12981,1.);
#3743=VECTOR('',#12990,1.);
#3744=VECTOR('',#12993,0.165);
#3745=VECTOR('',#12998,1.);
#3746=VECTOR('',#13009,1.);
#3747=VECTOR('',#13012,1.);
#3748=VECTOR('',#13013,0.165);
#3749=VECTOR('',#13026,1.);
#3750=VECTOR('',#13029,1.);
#3751=VECTOR('',#13030,0.165);
#3752=VECTOR('',#13037,1.5);
#3753=VECTOR('',#13052,1.05);
#3754=VECTOR('',#13067,2.);
#3755=VECTOR('',#13070,0.625);
#3756=VECTOR('',#13087,1.);
#3757=VECTOR('',#13090,0.165);
#3758=VECTOR('',#13095,1.);
#3759=VECTOR('',#13104,1.);
#3760=VECTOR('',#13107,0.165);
#3761=VECTOR('',#13112,1.);
#3762=VECTOR('',#13123,1.);
#3763=VECTOR('',#13126,1.);
#3764=VECTOR('',#13127,0.165);
#3765=VECTOR('',#13140,1.);
#3766=VECTOR('',#13143,1.);
#3767=VECTOR('',#13144,0.165);
#3768=VECTOR('',#13151,1.5);
#3769=VECTOR('',#13166,1.05);
#3770=VECTOR('',#13181,2.);
#3771=VECTOR('',#13184,0.625);
#3772=VECTOR('',#13201,1.);
#3773=VECTOR('',#13204,0.165);
#3774=VECTOR('',#13209,1.);
#3775=VECTOR('',#13218,1.);
#3776=VECTOR('',#13221,0.165);
#3777=VECTOR('',#13226,1.);
#3778=VECTOR('',#13237,1.);
#3779=VECTOR('',#13240,1.);
#3780=VECTOR('',#13241,0.165);
#3781=VECTOR('',#13254,1.);
#3782=VECTOR('',#13257,1.);
#3783=VECTOR('',#13258,0.165);
#3784=VECTOR('',#13265,1.5);
#3785=VECTOR('',#13280,1.05);
#3786=VECTOR('',#13295,2.);
#3787=VECTOR('',#13298,0.625);
#3788=VECTOR('',#13315,1.);
#3789=VECTOR('',#13318,0.165);
#3790=VECTOR('',#13323,1.);
#3791=VECTOR('',#13332,1.);
#3792=VECTOR('',#13335,0.165);
#3793=VECTOR('',#13340,1.);
#3794=VECTOR('',#13351,1.);
#3795=VECTOR('',#13354,1.);
#3796=VECTOR('',#13355,0.165);
#3797=VECTOR('',#13368,1.);
#3798=VECTOR('',#13371,1.);
#3799=VECTOR('',#13372,0.165);
#3800=VECTOR('',#13379,1.5);
#3801=VECTOR('',#13394,1.05);
#3802=VECTOR('',#13409,2.);
#3803=VECTOR('',#13412,0.625);
#3804=VECTOR('',#13425,0.165);
#3805=VECTOR('',#13432,0.165);
#3806=VECTOR('',#13439,0.165);
#3807=VECTOR('',#13446,0.165);
#3808=VECTOR('',#13459,1.5);
#3809=VECTOR('',#13462,0.5);
#3810=VECTOR('',#13477,1.);
#3811=VECTOR('',#13478,1.);
#3812=VECTOR('',#13479,1.);
#3813=VECTOR('',#13482,1.);
#3814=VECTOR('',#13483,1.);
#3815=VECTOR('',#13484,1.);
#3816=VECTOR('',#13489,1.);
#3817=VECTOR('',#13490,1.);
#3818=VECTOR('',#13493,1.);
#3819=VECTOR('',#13494,1.);
#3820=VECTOR('',#13507,1.05);
#3821=VECTOR('',#13516,1.);
#3822=VECTOR('',#13525,1.05);
#3823=VECTOR('',#13534,1.);
#3824=VECTOR('',#13543,1.05);
#3825=VECTOR('',#13550,0.9);
#3826=VECTOR('',#13557,1.);
#3827=VECTOR('',#13560,1.);
#3828=VECTOR('',#13563,1.);
#3829=VECTOR('',#13564,1.);
#3830=VECTOR('',#13565,1.);
#3831=VECTOR('',#13572,1.);
#3832=VECTOR('',#13575,1.);
#3833=VECTOR('',#13576,1.);
#3834=VECTOR('',#13587,0.895);
#3835=VECTOR('',#13594,0.605);
#3836=VECTOR('',#13609,0.325);
#3837=VECTOR('',#13614,0.35);
#3838=VECTOR('',#13619,0.335);
#3839=VECTOR('',#13628,0.21);
#3840=VECTOR('',#13633,0.2);
#3841=VECTOR('',#13638,0.18);
#3842=VECTOR('',#13643,1.);
#3843=VECTOR('',#13644,1.);
#3844=VECTOR('',#13645,1.);
#3845=VECTOR('',#13646,1.);
#3846=VECTOR('',#13649,1.);
#3847=VECTOR('',#13650,1.);
#3848=VECTOR('',#13651,1.);
#3849=VECTOR('',#13654,1.);
#3850=VECTOR('',#13655,1.);
#3851=VECTOR('',#13656,1.);
#3852=VECTOR('',#13659,1.);
#3853=VECTOR('',#13660,1.);
#3854=VECTOR('',#13661,1.);
#3855=VECTOR('',#13664,1.);
#3856=VECTOR('',#13665,1.);
#3857=VECTOR('',#13666,1.);
#3858=VECTOR('',#13669,1.);
#3859=VECTOR('',#13670,1.);
#3860=CIRCLE('',#9764,0.275);
#3861=CIRCLE('',#9765,0.275);
#3862=CIRCLE('',#9767,0.275);
#3863=CIRCLE('',#9768,0.275);
#3864=CIRCLE('',#9770,0.5);
#3865=CIRCLE('',#9771,0.5);
#3866=CIRCLE('',#9773,0.5);
#3867=CIRCLE('',#9774,0.5);
#3868=CIRCLE('',#9776,0.5);
#3869=CIRCLE('',#9777,0.5);
#3870=CIRCLE('',#9779,0.5);
#3871=CIRCLE('',#9780,0.5);
#3872=CIRCLE('',#9782,0.21);
#3873=CIRCLE('',#9783,0.21);
#3874=CIRCLE('',#9785,0.21);
#3875=CIRCLE('',#9786,0.21);
#3876=CIRCLE('',#9788,0.21);
#3877=CIRCLE('',#9789,0.21);
#3878=CIRCLE('',#9791,0.21);
#3879=CIRCLE('',#9792,0.21);
#3880=CIRCLE('',#9794,0.275);
#3881=CIRCLE('',#9795,0.275);
#3882=CIRCLE('',#9797,0.275);
#3883=CIRCLE('',#9798,0.275);
#3884=CIRCLE('',#9800,0.275);
#3885=CIRCLE('',#9801,0.275);
#3886=CIRCLE('',#9803,0.275);
#3887=CIRCLE('',#9804,0.275);
#3888=CIRCLE('',#9806,0.275);
#3889=CIRCLE('',#9807,0.275);
#3890=CIRCLE('',#9809,0.275);
#3891=CIRCLE('',#9810,0.275);
#3892=CIRCLE('',#9812,0.275);
#3893=CIRCLE('',#9813,0.275);
#3894=CIRCLE('',#9815,0.275);
#3895=CIRCLE('',#9816,0.275);
#3896=CIRCLE('',#9818,0.275);
#3897=CIRCLE('',#9819,0.275);
#3898=CIRCLE('',#9821,0.275);
#3899=CIRCLE('',#9822,0.275);
#3900=CIRCLE('',#9824,0.275);
#3901=CIRCLE('',#9825,0.275);
#3902=CIRCLE('',#9827,0.275);
#3903=CIRCLE('',#9828,0.275);
#3904=CIRCLE('',#9851,0.275);
#3905=CIRCLE('',#9852,0.275);
#3906=CIRCLE('',#9854,0.275);
#3907=CIRCLE('',#9855,0.275);
#3908=CIRCLE('',#9857,0.275);
#3909=CIRCLE('',#9858,0.275);
#3910=CIRCLE('',#9860,0.275);
#3911=CIRCLE('',#9861,0.275);
#3912=CIRCLE('',#9863,0.275);
#3913=CIRCLE('',#9864,0.275);
#3914=CIRCLE('',#9866,0.275);
#3915=CIRCLE('',#9867,0.275);
#3916=CIRCLE('',#9869,0.275);
#3917=CIRCLE('',#9870,0.275);
#3918=CIRCLE('',#9872,0.275);
#3919=CIRCLE('',#9873,0.275);
#3920=CIRCLE('',#9875,0.275);
#3921=CIRCLE('',#9876,0.275);
#3922=CIRCLE('',#9878,0.275);
#3923=CIRCLE('',#9879,0.275);
#3924=CIRCLE('',#9881,0.275);
#3925=CIRCLE('',#9882,0.275);
#3926=CIRCLE('',#9884,0.275);
#3927=CIRCLE('',#9885,0.275);
#3928=CIRCLE('',#9887,0.275);
#3929=CIRCLE('',#9888,0.275);
#3930=CIRCLE('',#9890,0.275);
#3931=CIRCLE('',#9891,0.275);
#3932=CIRCLE('',#9893,0.61);
#3933=CIRCLE('',#9894,0.61);
#3934=CIRCLE('',#9896,0.61);
#3935=CIRCLE('',#9897,0.61);
#3936=CIRCLE('',#9899,0.61);
#3937=CIRCLE('',#9900,0.61);
#3938=CIRCLE('',#9902,0.61);
#3939=CIRCLE('',#9903,0.61);
#3940=CIRCLE('',#9912,0.210000000000001);
#3941=CIRCLE('',#9913,0.210000000000001);
#3942=CIRCLE('',#9916,0.210000000000001);
#3943=CIRCLE('',#9917,0.210000000000001);
#3944=CIRCLE('',#9920,0.210000000000001);
#3945=CIRCLE('',#9921,0.210000000000001);
#3946=CIRCLE('',#9924,0.210000000000001);
#3947=CIRCLE('',#9925,0.210000000000001);
#3948=CIRCLE('',#9935,0.210000000000001);
#3949=CIRCLE('',#9936,0.210000000000001);
#3950=CIRCLE('',#9939,0.210000000000001);
#3951=CIRCLE('',#9940,0.210000000000001);
#3952=CIRCLE('',#9943,0.210000000000001);
#3953=CIRCLE('',#9944,0.210000000000001);
#3954=CIRCLE('',#9947,0.210000000000001);
#3955=CIRCLE('',#9948,0.210000000000001);
#3956=CIRCLE('',#9958,0.21);
#3957=CIRCLE('',#9959,0.21);
#3958=CIRCLE('',#9962,0.21);
#3959=CIRCLE('',#9963,0.21);
#3960=CIRCLE('',#9966,0.21);
#3961=CIRCLE('',#9967,0.21);
#3962=CIRCLE('',#9969,0.21);
#3963=CIRCLE('',#9970,0.21);
#3964=CIRCLE('',#9979,0.21);
#3965=CIRCLE('',#9980,0.21);
#3966=CIRCLE('',#9982,0.21);
#3967=CIRCLE('',#9983,0.21);
#3968=CIRCLE('',#9985,0.21);
#3969=CIRCLE('',#9986,0.21);
#3970=CIRCLE('',#9987,0.21);
#3971=CIRCLE('',#9988,0.21);
#3972=CIRCLE('',#9991,0.21);
#3973=CIRCLE('',#9992,0.21);
#3974=CIRCLE('',#9993,0.21);
#3975=CIRCLE('',#9994,0.21);
#3976=CIRCLE('',#10006,0.625);
#3977=CIRCLE('',#10007,0.625);
#3978=CIRCLE('',#10009,1.5);
#3979=CIRCLE('',#10010,1.5);
#3980=CIRCLE('',#10014,0.1);
#3981=CIRCLE('',#10015,0.1);
#3982=CIRCLE('',#10020,0.21);
#3983=CIRCLE('',#10021,0.21);
#3984=CIRCLE('',#10024,0.21);
#3985=CIRCLE('',#10025,0.21);
#3986=CIRCLE('',#10028,0.21);
#3987=CIRCLE('',#10029,0.21);
#3988=CIRCLE('',#10031,0.21);
#3989=CIRCLE('',#10032,0.21);
#3990=CIRCLE('',#10041,0.21);
#3991=CIRCLE('',#10042,0.21);
#3992=CIRCLE('',#10044,0.21);
#3993=CIRCLE('',#10045,0.21);
#3994=CIRCLE('',#10047,0.21);
#3995=CIRCLE('',#10048,0.21);
#3996=CIRCLE('',#10049,0.21);
#3997=CIRCLE('',#10050,0.21);
#3998=CIRCLE('',#10053,0.21);
#3999=CIRCLE('',#10054,0.21);
#4000=CIRCLE('',#10055,0.21);
#4001=CIRCLE('',#10056,0.21);
#4002=CIRCLE('',#10068,0.625);
#4003=CIRCLE('',#10069,0.625);
#4004=CIRCLE('',#10071,1.5);
#4005=CIRCLE('',#10072,1.5);
#4006=CIRCLE('',#10076,0.1);
#4007=CIRCLE('',#10077,0.1);
#4008=CIRCLE('',#10082,0.21);
#4009=CIRCLE('',#10083,0.21);
#4010=CIRCLE('',#10086,0.21);
#4011=CIRCLE('',#10087,0.21);
#4012=CIRCLE('',#10090,0.21);
#4013=CIRCLE('',#10091,0.21);
#4014=CIRCLE('',#10093,0.21);
#4015=CIRCLE('',#10094,0.21);
#4016=CIRCLE('',#10103,0.21);
#4017=CIRCLE('',#10104,0.21);
#4018=CIRCLE('',#10106,0.21);
#4019=CIRCLE('',#10107,0.21);
#4020=CIRCLE('',#10109,0.21);
#4021=CIRCLE('',#10110,0.21);
#4022=CIRCLE('',#10111,0.21);
#4023=CIRCLE('',#10112,0.21);
#4024=CIRCLE('',#10115,0.21);
#4025=CIRCLE('',#10116,0.21);
#4026=CIRCLE('',#10117,0.21);
#4027=CIRCLE('',#10118,0.21);
#4028=CIRCLE('',#10130,0.625);
#4029=CIRCLE('',#10131,0.625);
#4030=CIRCLE('',#10133,1.5);
#4031=CIRCLE('',#10134,1.5);
#4032=CIRCLE('',#10138,0.1);
#4033=CIRCLE('',#10139,0.1);
#4034=CIRCLE('',#10144,0.21);
#4035=CIRCLE('',#10145,0.21);
#4036=CIRCLE('',#10148,0.21);
#4037=CIRCLE('',#10149,0.21);
#4038=CIRCLE('',#10152,0.21);
#4039=CIRCLE('',#10153,0.21);
#4040=CIRCLE('',#10155,0.21);
#4041=CIRCLE('',#10156,0.21);
#4042=CIRCLE('',#10165,0.21);
#4043=CIRCLE('',#10166,0.21);
#4044=CIRCLE('',#10168,0.21);
#4045=CIRCLE('',#10169,0.21);
#4046=CIRCLE('',#10171,0.21);
#4047=CIRCLE('',#10172,0.21);
#4048=CIRCLE('',#10173,0.21);
#4049=CIRCLE('',#10174,0.21);
#4050=CIRCLE('',#10177,0.21);
#4051=CIRCLE('',#10178,0.21);
#4052=CIRCLE('',#10179,0.21);
#4053=CIRCLE('',#10180,0.21);
#4054=CIRCLE('',#10192,0.625);
#4055=CIRCLE('',#10193,0.625);
#4056=CIRCLE('',#10195,1.5);
#4057=CIRCLE('',#10196,1.5);
#4058=CIRCLE('',#10200,0.1);
#4059=CIRCLE('',#10201,0.1);
#4060=CIRCLE('',#10206,0.21);
#4061=CIRCLE('',#10207,0.21);
#4062=CIRCLE('',#10210,0.21);
#4063=CIRCLE('',#10211,0.21);
#4064=CIRCLE('',#10214,0.21);
#4065=CIRCLE('',#10215,0.21);
#4066=CIRCLE('',#10218,0.21);
#4067=CIRCLE('',#10219,0.21);
#4068=CIRCLE('',#10222,0.6);
#4069=CIRCLE('',#10223,0.6);
#4070=CIRCLE('',#10226,0.8);
#4071=CIRCLE('',#10227,0.8);
#4072=CIRCLE('',#10237,0.275);
#4073=CIRCLE('',#10238,0.275);
#4074=CIRCLE('',#10240,0.275);
#4075=CIRCLE('',#10241,0.275);
#4076=CIRCLE('',#10243,0.275);
#4077=CIRCLE('',#10244,0.275);
#4078=CIRCLE('',#10246,0.275);
#4079=CIRCLE('',#10247,0.275);
#4080=CIRCLE('',#10249,0.275);
#4081=CIRCLE('',#10250,0.275);
#4082=CIRCLE('',#10252,0.275);
#4083=CIRCLE('',#10253,0.275);
#4084=CIRCLE('',#10255,0.275);
#4085=CIRCLE('',#10256,0.275);
#4086=CIRCLE('',#10258,0.275);
#4087=CIRCLE('',#10259,0.275);
#4088=CIRCLE('',#10268,0.51);
#4089=CIRCLE('',#10269,0.51);
#4090=CIRCLE('',#10271,0.8);
#4091=CIRCLE('',#10272,0.8);
#4092=CIRCLE('',#10277,0.21);
#4093=CIRCLE('',#10278,0.21);
#4094=CIRCLE('',#10281,0.5);
#4095=CIRCLE('',#10282,0.5);
#4096=CIRCLE('',#10287,0.5);
#4097=CIRCLE('',#10288,0.5);
#4098=CIRCLE('',#10293,0.21);
#4099=CIRCLE('',#10294,0.21);
#4100=CIRCLE('',#10297,0.5);
#4101=CIRCLE('',#10298,0.5);
#4102=CIRCLE('',#10303,0.5);
#4103=CIRCLE('',#10304,0.5);
#4104=CIRCLE('',#10309,0.21);
#4105=CIRCLE('',#10310,0.21);
#4106=CIRCLE('',#10313,0.5);
#4107=CIRCLE('',#10314,0.5);
#4108=CIRCLE('',#10319,0.5);
#4109=CIRCLE('',#10320,0.5);
#4110=CIRCLE('',#10325,0.21);
#4111=CIRCLE('',#10326,0.21);
#4112=CIRCLE('',#10329,0.5);
#4113=CIRCLE('',#10330,0.5);
#4114=CIRCLE('',#10335,0.5);
#4115=CIRCLE('',#10336,0.5);
#4116=CIRCLE('',#10341,0.6);
#4117=CIRCLE('',#10342,0.5);
#4118=CIRCLE('',#10344,0.6);
#4119=CIRCLE('',#10347,0.5);
#4120=CIRCLE('',#10351,0.525);
#4121=CIRCLE('',#10353,0.525);
#4122=CIRCLE('',#10355,0.525);
#4123=CIRCLE('',#10356,0.525);
#4124=CIRCLE('',#10359,0.275);
#4125=CIRCLE('',#10361,0.165);
#4126=CIRCLE('',#10363,0.275);
#4127=CIRCLE('',#10365,0.225);
#4128=CIRCLE('',#10366,0.225);
#4129=CIRCLE('',#10368,0.165);
#4130=CIRCLE('',#10370,0.275);
#4131=CIRCLE('',#10372,0.275);
#4132=CIRCLE('',#10374,0.6);
#4133=CIRCLE('',#10375,0.6);
#4134=CIRCLE('',#10397,0.24505);
#4135=CIRCLE('',#10399,0.375);
#4136=CIRCLE('',#10401,0.425);
#4137=CIRCLE('',#10403,0.425);
#4138=CIRCLE('',#10405,0.395);
#4139=CIRCLE('',#10407,0.27);
#4140=CIRCLE('',#10409,0.24505);
#4141=CIRCLE('',#10413,0.375);
#4142=CIRCLE('',#10415,0.425);
#4143=CIRCLE('',#10417,0.425);
#4144=CIRCLE('',#10419,0.395);
#4145=CIRCLE('',#10421,0.27);
#4146=CIRCLE('',#10423,0.24505);
#4147=CIRCLE('',#10425,0.24505);
#4148=CIRCLE('',#10427,0.2);
#4149=CIRCLE('',#10440,0.225);
#4150=CIRCLE('',#10441,0.225);
#4151=CIRCLE('',#10443,0.225);
#4152=CIRCLE('',#10444,0.225);
#4153=CIRCLE('',#10446,0.225);
#4154=CIRCLE('',#10447,0.225);
#4155=CIRCLE('',#10449,0.225);
#4156=CIRCLE('',#10450,0.225);
#4157=CIRCLE('',#10452,0.225);
#4158=CIRCLE('',#10453,0.225);
#4159=CIRCLE('',#10455,0.225);
#4160=CIRCLE('',#10456,0.225);
#4161=CIRCLE('',#10458,0.225);
#4162=CIRCLE('',#10459,0.225);
#4163=CIRCLE('',#10461,0.225);
#4164=CIRCLE('',#10462,0.225);
#4165=CIRCLE('',#10464,0.225);
#4166=CIRCLE('',#10465,0.225);
#4167=CIRCLE('',#10467,0.225);
#4168=CIRCLE('',#10468,0.225);
#4169=CIRCLE('',#10470,0.225);
#4170=CIRCLE('',#10471,0.225);
#4171=CIRCLE('',#10473,0.225);
#4172=CIRCLE('',#10474,0.225);
#4173=CIRCLE('',#10476,0.225);
#4174=CIRCLE('',#10477,0.225);
#4175=CIRCLE('',#10479,0.225);
#4176=CIRCLE('',#10480,0.225);
#4177=CIRCLE('',#10482,0.225);
#4178=CIRCLE('',#10483,0.225);
#4179=CIRCLE('',#10485,0.225);
#4180=CIRCLE('',#10486,0.225);
#4181=CIRCLE('',#10488,0.225);
#4182=CIRCLE('',#10489,0.225);
#4183=CIRCLE('',#10491,0.225);
#4184=CIRCLE('',#10492,0.225);
#4185=CIRCLE('',#10494,0.225);
#4186=CIRCLE('',#10495,0.225);
#4187=CIRCLE('',#10497,0.225);
#4188=CIRCLE('',#10498,0.225);
#4189=CIRCLE('',#10500,0.625);
#4190=CIRCLE('',#10501,0.625);
#4191=CIRCLE('',#10503,0.625);
#4192=CIRCLE('',#10504,0.625);
#4193=CIRCLE('',#10506,0.625);
#4194=CIRCLE('',#10507,0.625);
#4195=CIRCLE('',#10509,0.625);
#4196=CIRCLE('',#10510,0.625);
#4197=CIRCLE('',#10519,1.5);
#4198=CIRCLE('',#10520,0.165);
#4199=CIRCLE('',#10522,0.165);
#4200=CIRCLE('',#10523,0.165);
#4201=CIRCLE('',#10524,0.165);
#4202=CIRCLE('',#10526,1.5);
#4203=CIRCLE('',#10527,0.165);
#4204=CIRCLE('',#10529,0.165);
#4205=CIRCLE('',#10530,0.165);
#4206=CIRCLE('',#10531,0.165);
#4207=CIRCLE('',#10533,1.5);
#4208=CIRCLE('',#10534,0.165);
#4209=CIRCLE('',#10535,0.165);
#4210=CIRCLE('',#10537,0.165);
#4211=CIRCLE('',#10538,0.165);
#4212=CIRCLE('',#10540,1.5);
#4213=CIRCLE('',#10541,0.165);
#4214=CIRCLE('',#10542,0.165);
#4215=CIRCLE('',#10544,0.165);
#4216=CIRCLE('',#10545,0.165);
#4217=CIRCLE('',#10547,1.5);
#4218=CIRCLE('',#10548,1.5);
#4219=CIRCLE('',#10549,1.5);
#4220=CIRCLE('',#10550,1.5);
#4221=CIRCLE('',#10551,1.5);
#4222=CIRCLE('',#10552,1.5);
#4223=CIRCLE('',#10554,1.05);
#4224=CIRCLE('',#10555,1.05);
#4225=CIRCLE('',#10557,0.625);
#4226=CIRCLE('',#10559,2.);
#4227=CIRCLE('',#10561,2.);
#4228=CIRCLE('',#10563,0.625);
#4229=CIRCLE('',#10568,1.5);
#4230=CIRCLE('',#10569,0.165);
#4231=CIRCLE('',#10571,0.165);
#4232=CIRCLE('',#10572,0.165);
#4233=CIRCLE('',#10573,0.165);
#4234=CIRCLE('',#10575,1.5);
#4235=CIRCLE('',#10576,0.165);
#4236=CIRCLE('',#10578,0.165);
#4237=CIRCLE('',#10579,0.165);
#4238=CIRCLE('',#10580,0.165);
#4239=CIRCLE('',#10582,1.5);
#4240=CIRCLE('',#10583,0.165);
#4241=CIRCLE('',#10584,0.165);
#4242=CIRCLE('',#10586,0.165);
#4243=CIRCLE('',#10587,0.165);
#4244=CIRCLE('',#10589,1.5);
#4245=CIRCLE('',#10590,0.165);
#4246=CIRCLE('',#10591,0.165);
#4247=CIRCLE('',#10593,0.165);
#4248=CIRCLE('',#10594,0.165);
#4249=CIRCLE('',#10596,1.5);
#4250=CIRCLE('',#10597,1.5);
#4251=CIRCLE('',#10598,1.5);
#4252=CIRCLE('',#10599,1.5);
#4253=CIRCLE('',#10600,1.5);
#4254=CIRCLE('',#10601,1.5);
#4255=CIRCLE('',#10603,1.05);
#4256=CIRCLE('',#10604,1.05);
#4257=CIRCLE('',#10606,0.625);
#4258=CIRCLE('',#10608,2.);
#4259=CIRCLE('',#10610,2.);
#4260=CIRCLE('',#10612,0.625);
#4261=CIRCLE('',#10617,1.5);
#4262=CIRCLE('',#10618,0.165);
#4263=CIRCLE('',#10620,0.165);
#4264=CIRCLE('',#10621,0.165);
#4265=CIRCLE('',#10622,0.165);
#4266=CIRCLE('',#10624,1.5);
#4267=CIRCLE('',#10625,0.165);
#4268=CIRCLE('',#10627,0.165);
#4269=CIRCLE('',#10628,0.165);
#4270=CIRCLE('',#10629,0.165);
#4271=CIRCLE('',#10631,1.5);
#4272=CIRCLE('',#10632,0.165);
#4273=CIRCLE('',#10633,0.165);
#4274=CIRCLE('',#10635,0.165);
#4275=CIRCLE('',#10636,0.165);
#4276=CIRCLE('',#10638,1.5);
#4277=CIRCLE('',#10639,0.165);
#4278=CIRCLE('',#10640,0.165);
#4279=CIRCLE('',#10642,0.165);
#4280=CIRCLE('',#10643,0.165);
#4281=CIRCLE('',#10645,1.5);
#4282=CIRCLE('',#10646,1.5);
#4283=CIRCLE('',#10647,1.5);
#4284=CIRCLE('',#10648,1.5);
#4285=CIRCLE('',#10649,1.5);
#4286=CIRCLE('',#10650,1.5);
#4287=CIRCLE('',#10652,1.05);
#4288=CIRCLE('',#10653,1.05);
#4289=CIRCLE('',#10655,0.625);
#4290=CIRCLE('',#10657,2.);
#4291=CIRCLE('',#10659,2.);
#4292=CIRCLE('',#10661,0.625);
#4293=CIRCLE('',#10666,1.5);
#4294=CIRCLE('',#10667,0.165);
#4295=CIRCLE('',#10669,0.165);
#4296=CIRCLE('',#10670,0.165);
#4297=CIRCLE('',#10671,0.165);
#4298=CIRCLE('',#10673,1.5);
#4299=CIRCLE('',#10674,0.165);
#4300=CIRCLE('',#10676,0.165);
#4301=CIRCLE('',#10677,0.165);
#4302=CIRCLE('',#10678,0.165);
#4303=CIRCLE('',#10680,1.5);
#4304=CIRCLE('',#10681,0.165);
#4305=CIRCLE('',#10682,0.165);
#4306=CIRCLE('',#10684,0.165);
#4307=CIRCLE('',#10685,0.165);
#4308=CIRCLE('',#10687,1.5);
#4309=CIRCLE('',#10688,0.165);
#4310=CIRCLE('',#10689,0.165);
#4311=CIRCLE('',#10691,0.165);
#4312=CIRCLE('',#10692,0.165);
#4313=CIRCLE('',#10694,1.5);
#4314=CIRCLE('',#10695,1.5);
#4315=CIRCLE('',#10696,1.5);
#4316=CIRCLE('',#10697,1.5);
#4317=CIRCLE('',#10698,1.5);
#4318=CIRCLE('',#10699,1.5);
#4319=CIRCLE('',#10701,1.05);
#4320=CIRCLE('',#10702,1.05);
#4321=CIRCLE('',#10704,0.625);
#4322=CIRCLE('',#10706,2.);
#4323=CIRCLE('',#10708,2.);
#4324=CIRCLE('',#10710,0.625);
#4325=CIRCLE('',#10715,0.165);
#4326=CIRCLE('',#10716,0.165);
#4327=CIRCLE('',#10718,0.165);
#4328=CIRCLE('',#10719,0.165);
#4329=CIRCLE('',#10721,0.165);
#4330=CIRCLE('',#10722,0.165);
#4331=CIRCLE('',#10724,0.165);
#4332=CIRCLE('',#10725,0.165);
#4333=CIRCLE('',#10727,1.5);
#4334=CIRCLE('',#10728,0.5);
#4335=CIRCLE('',#10730,1.5);
#4336=CIRCLE('',#10732,0.5);
#4337=CIRCLE('',#10738,0.9);
#4338=CIRCLE('',#10741,0.9);
#4339=CIRCLE('',#10745,1.05);
#4340=CIRCLE('',#10746,0.9);
#4341=CIRCLE('',#10748,1.05);
#4342=CIRCLE('',#10750,1.);
#4343=CIRCLE('',#10752,1.);
#4344=CIRCLE('',#10754,1.05);
#4345=CIRCLE('',#10756,1.05);
#4346=CIRCLE('',#10758,1.);
#4347=CIRCLE('',#10760,1.);
#4348=CIRCLE('',#10762,1.05);
#4349=CIRCLE('',#10764,1.05);
#4350=CIRCLE('',#10766,0.9);
#4351=CIRCLE('',#10770,0.895);
#4352=CIRCLE('',#10771,0.605);
#4353=CIRCLE('',#10774,0.895);
#4354=CIRCLE('',#10775,0.605);
#4355=CIRCLE('',#10778,0.895);
#4356=CIRCLE('',#10779,0.605);
#4357=CIRCLE('',#10781,0.895);
#4358=CIRCLE('',#10783,0.605);
#4359=CIRCLE('',#10789,0.3);
#4360=CIRCLE('',#10791,0.35);
#4361=CIRCLE('',#10793,0.35);
#4362=CIRCLE('',#10795,0.32);
#4363=CIRCLE('',#10797,0.22);
#4364=CIRCLE('',#10799,0.1954);
#4365=CIRCLE('',#10801,0.1954);
#4366=CIRCLE('',#10803,0.16);
#4367=VERTEX_POINT('',#13953);
#4368=VERTEX_POINT('',#13955);
#4369=VERTEX_POINT('',#13959);
#4370=VERTEX_POINT('',#13961);
#4371=VERTEX_POINT('',#13965);
#4372=VERTEX_POINT('',#13967);
#4373=VERTEX_POINT('',#13971);
#4374=VERTEX_POINT('',#13973);
#4375=VERTEX_POINT('',#13977);
#4376=VERTEX_POINT('',#13979);
#4377=VERTEX_POINT('',#13983);
#4378=VERTEX_POINT('',#13985);
#4379=VERTEX_POINT('',#13989);
#4380=VERTEX_POINT('',#13991);
#4381=VERTEX_POINT('',#13995);
#4382=VERTEX_POINT('',#13997);
#4383=VERTEX_POINT('',#14001);
#4384=VERTEX_POINT('',#14003);
#4385=VERTEX_POINT('',#14007);
#4386=VERTEX_POINT('',#14009);
#4387=VERTEX_POINT('',#14013);
#4388=VERTEX_POINT('',#14015);
#4389=VERTEX_POINT('',#14019);
#4390=VERTEX_POINT('',#14021);
#4391=VERTEX_POINT('',#14025);
#4392=VERTEX_POINT('',#14027);
#4393=VERTEX_POINT('',#14031);
#4394=VERTEX_POINT('',#14033);
#4395=VERTEX_POINT('',#14037);
#4396=VERTEX_POINT('',#14039);
#4397=VERTEX_POINT('',#14043);
#4398=VERTEX_POINT('',#14045);
#4399=VERTEX_POINT('',#14049);
#4400=VERTEX_POINT('',#14051);
#4401=VERTEX_POINT('',#14055);
#4402=VERTEX_POINT('',#14057);
#4403=VERTEX_POINT('',#14061);
#4404=VERTEX_POINT('',#14063);
#4405=VERTEX_POINT('',#14067);
#4406=VERTEX_POINT('',#14069);
#4407=VERTEX_POINT('',#14073);
#4408=VERTEX_POINT('',#14075);
#4409=VERTEX_POINT('',#14079);
#4410=VERTEX_POINT('',#14081);
#4411=VERTEX_POINT('',#14085);
#4412=VERTEX_POINT('',#14086);
#4413=VERTEX_POINT('',#14088);
#4414=VERTEX_POINT('',#14090);
#4415=VERTEX_POINT('',#14094);
#4416=VERTEX_POINT('',#14096);
#4417=VERTEX_POINT('',#14100);
#4418=VERTEX_POINT('',#14102);
#4419=VERTEX_POINT('',#14112);
#4420=VERTEX_POINT('',#14113);
#4421=VERTEX_POINT('',#14115);
#4422=VERTEX_POINT('',#14117);
#4423=VERTEX_POINT('',#14121);
#4424=VERTEX_POINT('',#14123);
#4425=VERTEX_POINT('',#14127);
#4426=VERTEX_POINT('',#14129);
#4427=VERTEX_POINT('',#14139);
#4428=VERTEX_POINT('',#14140);
#4429=VERTEX_POINT('',#14142);
#4430=VERTEX_POINT('',#14144);
#4431=VERTEX_POINT('',#14148);
#4432=VERTEX_POINT('',#14150);
#4433=VERTEX_POINT('',#14154);
#4434=VERTEX_POINT('',#14156);
#4435=VERTEX_POINT('',#14166);
#4436=VERTEX_POINT('',#14168);
#4437=VERTEX_POINT('',#14172);
#4438=VERTEX_POINT('',#14174);
#4439=VERTEX_POINT('',#14178);
#4440=VERTEX_POINT('',#14180);
#4441=VERTEX_POINT('',#14184);
#4442=VERTEX_POINT('',#14186);
#4443=VERTEX_POINT('',#14190);
#4444=VERTEX_POINT('',#14192);
#4445=VERTEX_POINT('',#14196);
#4446=VERTEX_POINT('',#14198);
#4447=VERTEX_POINT('',#14202);
#4448=VERTEX_POINT('',#14204);
#4449=VERTEX_POINT('',#14208);
#4450=VERTEX_POINT('',#14210);
#4451=VERTEX_POINT('',#14214);
#4452=VERTEX_POINT('',#14216);
#4453=VERTEX_POINT('',#14220);
#4454=VERTEX_POINT('',#14222);
#4455=VERTEX_POINT('',#14226);
#4456=VERTEX_POINT('',#14228);
#4457=VERTEX_POINT('',#14232);
#4458=VERTEX_POINT('',#14234);
#4459=VERTEX_POINT('',#14238);
#4460=VERTEX_POINT('',#14240);
#4461=VERTEX_POINT('',#14244);
#4462=VERTEX_POINT('',#14246);
#4463=VERTEX_POINT('',#14250);
#4464=VERTEX_POINT('',#14252);
#4465=VERTEX_POINT('',#14256);
#4466=VERTEX_POINT('',#14258);
#4467=VERTEX_POINT('',#14262);
#4468=VERTEX_POINT('',#14264);
#4469=VERTEX_POINT('',#14268);
#4470=VERTEX_POINT('',#14270);
#4471=VERTEX_POINT('',#14274);
#4472=VERTEX_POINT('',#14275);
#4473=VERTEX_POINT('',#14277);
#4474=VERTEX_POINT('',#14279);
#4475=VERTEX_POINT('',#14283);
#4476=VERTEX_POINT('',#14285);
#4477=VERTEX_POINT('',#14289);
#4478=VERTEX_POINT('',#14291);
#4479=VERTEX_POINT('',#14301);
#4480=VERTEX_POINT('',#14303);
#4481=VERTEX_POINT('',#14308);
#4482=VERTEX_POINT('',#14310);
#4483=VERTEX_POINT('',#14315);
#4484=VERTEX_POINT('',#14317);
#4485=VERTEX_POINT('',#14322);
#4486=VERTEX_POINT('',#14324);
#4487=VERTEX_POINT('',#14329);
#4488=VERTEX_POINT('',#14330);
#4489=VERTEX_POINT('',#14332);
#4490=VERTEX_POINT('',#14334);
#4491=VERTEX_POINT('',#14338);
#4492=VERTEX_POINT('',#14340);
#4493=VERTEX_POINT('',#14344);
#4494=VERTEX_POINT('',#14346);
#4495=VERTEX_POINT('',#14356);
#4496=VERTEX_POINT('',#14358);
#4497=VERTEX_POINT('',#14363);
#4498=VERTEX_POINT('',#14365);
#4499=VERTEX_POINT('',#14370);
#4500=VERTEX_POINT('',#14372);
#4501=VERTEX_POINT('',#14377);
#4502=VERTEX_POINT('',#14379);
#4503=VERTEX_POINT('',#14384);
#4504=VERTEX_POINT('',#14385);
#4505=VERTEX_POINT('',#14387);
#4506=VERTEX_POINT('',#14389);
#4507=VERTEX_POINT('',#14393);
#4508=VERTEX_POINT('',#14395);
#4509=VERTEX_POINT('',#14399);
#4510=VERTEX_POINT('',#14401);
#4511=VERTEX_POINT('',#14411);
#4512=VERTEX_POINT('',#14413);
#4513=VERTEX_POINT('',#14418);
#4514=VERTEX_POINT('',#14420);
#4515=VERTEX_POINT('',#14425);
#4516=VERTEX_POINT('',#14427);
#4517=VERTEX_POINT('',#14431);
#4518=VERTEX_POINT('',#14433);
#4519=VERTEX_POINT('',#14437);
#4520=VERTEX_POINT('',#14438);
#4521=VERTEX_POINT('',#14440);
#4522=VERTEX_POINT('',#14442);
#4523=VERTEX_POINT('',#14446);
#4524=VERTEX_POINT('',#14448);
#4525=VERTEX_POINT('',#14452);
#4526=VERTEX_POINT('',#14454);
#4527=VERTEX_POINT('',#14464);
#4528=VERTEX_POINT('',#14466);
#4529=VERTEX_POINT('',#14470);
#4530=VERTEX_POINT('',#14472);
#4531=VERTEX_POINT('',#14476);
#4532=VERTEX_POINT('',#14478);
#4533=VERTEX_POINT('',#14480);
#4534=VERTEX_POINT('',#14482);
#4535=VERTEX_POINT('',#14484);
#4536=VERTEX_POINT('',#14486);
#4537=VERTEX_POINT('',#14492);
#4538=VERTEX_POINT('',#14494);
#4539=VERTEX_POINT('',#14496);
#4540=VERTEX_POINT('',#14498);
#4541=VERTEX_POINT('',#14500);
#4542=VERTEX_POINT('',#14502);
#4543=VERTEX_POINT('',#14509);
#4544=VERTEX_POINT('',#14511);
#4545=VERTEX_POINT('',#14513);
#4546=VERTEX_POINT('',#14515);
#4547=VERTEX_POINT('',#14519);
#4548=VERTEX_POINT('',#14521);
#4549=VERTEX_POINT('',#14525);
#4550=VERTEX_POINT('',#14526);
#4551=VERTEX_POINT('',#14531);
#4552=VERTEX_POINT('',#14532);
#4553=VERTEX_POINT('',#14537);
#4554=VERTEX_POINT('',#14538);
#4555=VERTEX_POINT('',#14549);
#4556=VERTEX_POINT('',#14551);
#4557=VERTEX_POINT('',#14555);
#4558=VERTEX_POINT('',#14557);
#4559=VERTEX_POINT('',#15903);
#4560=VERTEX_POINT('',#15905);
#4561=VERTEX_POINT('',#16045);
#4562=VERTEX_POINT('',#16047);
#4563=VERTEX_POINT('',#16052);
#4564=VERTEX_POINT('',#16054);
#4565=VERTEX_POINT('',#16059);
#4566=VERTEX_POINT('',#16061);
#4567=VERTEX_POINT('',#16065);
#4568=VERTEX_POINT('',#16067);
#4569=VERTEX_POINT('',#16071);
#4570=VERTEX_POINT('',#16072);
#4571=VERTEX_POINT('',#16074);
#4572=VERTEX_POINT('',#16076);
#4573=VERTEX_POINT('',#16080);
#4574=VERTEX_POINT('',#16082);
#4575=VERTEX_POINT('',#16086);
#4576=VERTEX_POINT('',#16088);
#4577=VERTEX_POINT('',#16098);
#4578=VERTEX_POINT('',#16100);
#4579=VERTEX_POINT('',#16104);
#4580=VERTEX_POINT('',#16106);
#4581=VERTEX_POINT('',#16110);
#4582=VERTEX_POINT('',#16112);
#4583=VERTEX_POINT('',#16114);
#4584=VERTEX_POINT('',#16116);
#4585=VERTEX_POINT('',#16118);
#4586=VERTEX_POINT('',#16120);
#4587=VERTEX_POINT('',#16126);
#4588=VERTEX_POINT('',#16128);
#4589=VERTEX_POINT('',#16130);
#4590=VERTEX_POINT('',#16132);
#4591=VERTEX_POINT('',#16134);
#4592=VERTEX_POINT('',#16136);
#4593=VERTEX_POINT('',#16143);
#4594=VERTEX_POINT('',#16145);
#4595=VERTEX_POINT('',#16147);
#4596=VERTEX_POINT('',#16149);
#4597=VERTEX_POINT('',#16153);
#4598=VERTEX_POINT('',#16155);
#4599=VERTEX_POINT('',#16159);
#4600=VERTEX_POINT('',#16160);
#4601=VERTEX_POINT('',#16165);
#4602=VERTEX_POINT('',#16166);
#4603=VERTEX_POINT('',#16171);
#4604=VERTEX_POINT('',#16172);
#4605=VERTEX_POINT('',#16183);
#4606=VERTEX_POINT('',#16185);
#4607=VERTEX_POINT('',#16189);
#4608=VERTEX_POINT('',#16191);
#4609=VERTEX_POINT('',#17467);
#4610=VERTEX_POINT('',#17469);
#4611=VERTEX_POINT('',#17602);
#4612=VERTEX_POINT('',#17604);
#4613=VERTEX_POINT('',#17609);
#4614=VERTEX_POINT('',#17611);
#4615=VERTEX_POINT('',#17616);
#4616=VERTEX_POINT('',#17618);
#4617=VERTEX_POINT('',#17622);
#4618=VERTEX_POINT('',#17624);
#4619=VERTEX_POINT('',#17628);
#4620=VERTEX_POINT('',#17629);
#4621=VERTEX_POINT('',#17631);
#4622=VERTEX_POINT('',#17633);
#4623=VERTEX_POINT('',#17637);
#4624=VERTEX_POINT('',#17639);
#4625=VERTEX_POINT('',#17643);
#4626=VERTEX_POINT('',#17645);
#4627=VERTEX_POINT('',#17655);
#4628=VERTEX_POINT('',#17657);
#4629=VERTEX_POINT('',#17661);
#4630=VERTEX_POINT('',#17663);
#4631=VERTEX_POINT('',#17667);
#4632=VERTEX_POINT('',#17669);
#4633=VERTEX_POINT('',#17671);
#4634=VERTEX_POINT('',#17673);
#4635=VERTEX_POINT('',#17675);
#4636=VERTEX_POINT('',#17677);
#4637=VERTEX_POINT('',#17683);
#4638=VERTEX_POINT('',#17685);
#4639=VERTEX_POINT('',#17687);
#4640=VERTEX_POINT('',#17689);
#4641=VERTEX_POINT('',#17691);
#4642=VERTEX_POINT('',#17693);
#4643=VERTEX_POINT('',#17700);
#4644=VERTEX_POINT('',#17702);
#4645=VERTEX_POINT('',#17704);
#4646=VERTEX_POINT('',#17706);
#4647=VERTEX_POINT('',#17710);
#4648=VERTEX_POINT('',#17712);
#4649=VERTEX_POINT('',#17716);
#4650=VERTEX_POINT('',#17717);
#4651=VERTEX_POINT('',#17722);
#4652=VERTEX_POINT('',#17723);
#4653=VERTEX_POINT('',#17728);
#4654=VERTEX_POINT('',#17729);
#4655=VERTEX_POINT('',#17740);
#4656=VERTEX_POINT('',#17742);
#4657=VERTEX_POINT('',#17746);
#4658=VERTEX_POINT('',#17748);
#4659=VERTEX_POINT('',#19134);
#4660=VERTEX_POINT('',#19136);
#4661=VERTEX_POINT('',#19280);
#4662=VERTEX_POINT('',#19282);
#4663=VERTEX_POINT('',#19287);
#4664=VERTEX_POINT('',#19289);
#4665=VERTEX_POINT('',#19294);
#4666=VERTEX_POINT('',#19296);
#4667=VERTEX_POINT('',#19300);
#4668=VERTEX_POINT('',#19302);
#4669=VERTEX_POINT('',#19306);
#4670=VERTEX_POINT('',#19307);
#4671=VERTEX_POINT('',#19309);
#4672=VERTEX_POINT('',#19311);
#4673=VERTEX_POINT('',#19315);
#4674=VERTEX_POINT('',#19317);
#4675=VERTEX_POINT('',#19321);
#4676=VERTEX_POINT('',#19323);
#4677=VERTEX_POINT('',#19333);
#4678=VERTEX_POINT('',#19335);
#4679=VERTEX_POINT('',#19339);
#4680=VERTEX_POINT('',#19341);
#4681=VERTEX_POINT('',#19345);
#4682=VERTEX_POINT('',#19347);
#4683=VERTEX_POINT('',#19349);
#4684=VERTEX_POINT('',#19351);
#4685=VERTEX_POINT('',#19353);
#4686=VERTEX_POINT('',#19355);
#4687=VERTEX_POINT('',#19361);
#4688=VERTEX_POINT('',#19363);
#4689=VERTEX_POINT('',#19365);
#4690=VERTEX_POINT('',#19367);
#4691=VERTEX_POINT('',#19369);
#4692=VERTEX_POINT('',#19371);
#4693=VERTEX_POINT('',#19378);
#4694=VERTEX_POINT('',#19380);
#4695=VERTEX_POINT('',#19382);
#4696=VERTEX_POINT('',#19384);
#4697=VERTEX_POINT('',#19388);
#4698=VERTEX_POINT('',#19390);
#4699=VERTEX_POINT('',#19394);
#4700=VERTEX_POINT('',#19395);
#4701=VERTEX_POINT('',#19400);
#4702=VERTEX_POINT('',#19401);
#4703=VERTEX_POINT('',#19406);
#4704=VERTEX_POINT('',#19407);
#4705=VERTEX_POINT('',#19418);
#4706=VERTEX_POINT('',#19420);
#4707=VERTEX_POINT('',#19424);
#4708=VERTEX_POINT('',#19426);
#4709=VERTEX_POINT('',#20702);
#4710=VERTEX_POINT('',#20704);
#4711=VERTEX_POINT('',#20837);
#4712=VERTEX_POINT('',#20839);
#4713=VERTEX_POINT('',#20844);
#4714=VERTEX_POINT('',#20846);
#4715=VERTEX_POINT('',#20851);
#4716=VERTEX_POINT('',#20853);
#4717=VERTEX_POINT('',#20858);
#4718=VERTEX_POINT('',#20860);
#4719=VERTEX_POINT('',#20865);
#4720=VERTEX_POINT('',#20867);
#4721=VERTEX_POINT('',#20872);
#4722=VERTEX_POINT('',#20874);
#4723=VERTEX_POINT('',#20879);
#4724=VERTEX_POINT('',#20880);
#4725=VERTEX_POINT('',#20882);
#4726=VERTEX_POINT('',#20884);
#4727=VERTEX_POINT('',#20888);
#4728=VERTEX_POINT('',#20890);
#4729=VERTEX_POINT('',#20894);
#4730=VERTEX_POINT('',#20896);
#4731=VERTEX_POINT('',#20906);
#4732=VERTEX_POINT('',#20908);
#4733=VERTEX_POINT('',#20912);
#4734=VERTEX_POINT('',#20914);
#4735=VERTEX_POINT('',#20918);
#4736=VERTEX_POINT('',#20920);
#4737=VERTEX_POINT('',#20924);
#4738=VERTEX_POINT('',#20926);
#4739=VERTEX_POINT('',#20930);
#4740=VERTEX_POINT('',#20932);
#4741=VERTEX_POINT('',#20936);
#4742=VERTEX_POINT('',#20938);
#4743=VERTEX_POINT('',#20942);
#4744=VERTEX_POINT('',#20944);
#4745=VERTEX_POINT('',#20948);
#4746=VERTEX_POINT('',#20950);
#4747=VERTEX_POINT('',#20954);
#4748=VERTEX_POINT('',#20955);
#4749=VERTEX_POINT('',#20957);
#4750=VERTEX_POINT('',#20959);
#4751=VERTEX_POINT('',#20963);
#4752=VERTEX_POINT('',#20965);
#4753=VERTEX_POINT('',#20969);
#4754=VERTEX_POINT('',#20971);
#4755=VERTEX_POINT('',#20981);
#4756=VERTEX_POINT('',#20983);
#4757=VERTEX_POINT('',#20987);
#4758=VERTEX_POINT('',#20989);
#4759=VERTEX_POINT('',#20996);
#4760=VERTEX_POINT('',#20998);
#4761=VERTEX_POINT('',#21003);
#4762=VERTEX_POINT('',#21005);
#4763=VERTEX_POINT('',#21012);
#4764=VERTEX_POINT('',#21014);
#4765=VERTEX_POINT('',#21021);
#4766=VERTEX_POINT('',#21023);
#4767=VERTEX_POINT('',#21028);
#4768=VERTEX_POINT('',#21030);
#4769=VERTEX_POINT('',#21037);
#4770=VERTEX_POINT('',#21039);
#4771=VERTEX_POINT('',#21046);
#4772=VERTEX_POINT('',#21048);
#4773=VERTEX_POINT('',#21053);
#4774=VERTEX_POINT('',#21055);
#4775=VERTEX_POINT('',#21062);
#4776=VERTEX_POINT('',#21064);
#4777=VERTEX_POINT('',#21071);
#4778=VERTEX_POINT('',#21073);
#4779=VERTEX_POINT('',#21078);
#4780=VERTEX_POINT('',#21080);
#4781=VERTEX_POINT('',#21087);
#4782=VERTEX_POINT('',#21089);
#4783=VERTEX_POINT('',#21096);
#4784=VERTEX_POINT('',#21098);
#4785=VERTEX_POINT('',#21102);
#4786=VERTEX_POINT('',#21107);
#4787=VERTEX_POINT('',#21113);
#4788=VERTEX_POINT('',#21114);
#4789=VERTEX_POINT('',#21118);
#4790=VERTEX_POINT('',#21120);
#4791=VERTEX_POINT('',#21124);
#4792=VERTEX_POINT('',#21125);
#4793=VERTEX_POINT('',#21127);
#4794=VERTEX_POINT('',#21129);
#4795=VERTEX_POINT('',#21135);
#4796=VERTEX_POINT('',#21137);
#4797=VERTEX_POINT('',#21139);
#4798=VERTEX_POINT('',#21141);
#4799=VERTEX_POINT('',#21144);
#4800=VERTEX_POINT('',#21147);
#4801=VERTEX_POINT('',#21149);
#4802=VERTEX_POINT('',#21152);
#4803=VERTEX_POINT('',#21155);
#4804=VERTEX_POINT('',#21156);
#4805=VERTEX_POINT('',#21158);
#4806=VERTEX_POINT('',#21161);
#4807=VERTEX_POINT('',#21164);
#4808=VERTEX_POINT('',#21167);
#4809=VERTEX_POINT('',#21169);
#4810=VERTEX_POINT('',#21173);
#4811=VERTEX_POINT('',#21177);
#4812=VERTEX_POINT('',#21181);
#4813=VERTEX_POINT('',#21185);
#4814=VERTEX_POINT('',#21187);
#4815=VERTEX_POINT('',#21191);
#4816=VERTEX_POINT('',#21193);
#4817=VERTEX_POINT('',#21196);
#4818=VERTEX_POINT('',#21198);
#4819=VERTEX_POINT('',#21200);
#4820=VERTEX_POINT('',#21202);
#4821=VERTEX_POINT('',#21204);
#4822=VERTEX_POINT('',#21208);
#4823=VERTEX_POINT('',#21212);
#4824=VERTEX_POINT('',#21218);
#4825=VERTEX_POINT('',#21222);
#4826=VERTEX_POINT('',#21226);
#4827=VERTEX_POINT('',#21230);
#4828=VERTEX_POINT('',#21234);
#4829=VERTEX_POINT('',#21242);
#4830=VERTEX_POINT('',#21243);
#4831=VERTEX_POINT('',#21245);
#4832=VERTEX_POINT('',#21247);
#4833=VERTEX_POINT('',#21251);
#4834=VERTEX_POINT('',#21253);
#4835=VERTEX_POINT('',#21257);
#4836=VERTEX_POINT('',#21259);
#4837=VERTEX_POINT('',#21263);
#4838=VERTEX_POINT('',#21265);
#4839=VERTEX_POINT('',#21269);
#4840=VERTEX_POINT('',#21271);
#4841=VERTEX_POINT('',#21280);
#4842=VERTEX_POINT('',#21283);
#4843=VERTEX_POINT('',#21286);
#4844=VERTEX_POINT('',#21290);
#4845=VERTEX_POINT('',#21294);
#4846=VERTEX_POINT('',#21298);
#4847=VERTEX_POINT('',#21301);
#4848=VERTEX_POINT('',#21308);
#4849=VERTEX_POINT('',#21311);
#4850=VERTEX_POINT('',#21315);
#4851=VERTEX_POINT('',#21319);
#4852=VERTEX_POINT('',#21323);
#4853=VERTEX_POINT('',#21326);
#4854=VERTEX_POINT('',#21330);
#4855=VERTEX_POINT('',#21334);
#4856=VERTEX_POINT('',#21339);
#4857=VERTEX_POINT('',#21340);
#4858=VERTEX_POINT('',#21342);
#4859=VERTEX_POINT('',#21344);
#4860=VERTEX_POINT('',#21348);
#4861=VERTEX_POINT('',#21350);
#4862=VERTEX_POINT('',#21354);
#4863=VERTEX_POINT('',#21356);
#4864=VERTEX_POINT('',#21360);
#4865=VERTEX_POINT('',#21362);
#4866=VERTEX_POINT('',#21366);
#4867=VERTEX_POINT('',#21368);
#4868=VERTEX_POINT('',#21379);
#4869=VERTEX_POINT('',#21381);
#4870=VERTEX_POINT('',#21385);
#4871=VERTEX_POINT('',#21387);
#4872=VERTEX_POINT('',#21391);
#4873=VERTEX_POINT('',#21393);
#4874=VERTEX_POINT('',#21397);
#4875=VERTEX_POINT('',#21399);
#4876=VERTEX_POINT('',#21403);
#4877=VERTEX_POINT('',#21405);
#4878=VERTEX_POINT('',#21409);
#4879=VERTEX_POINT('',#21411);
#4880=VERTEX_POINT('',#21415);
#4881=VERTEX_POINT('',#21417);
#4882=VERTEX_POINT('',#21421);
#4883=VERTEX_POINT('',#21423);
#4884=VERTEX_POINT('',#21427);
#4885=VERTEX_POINT('',#21429);
#4886=VERTEX_POINT('',#21433);
#4887=VERTEX_POINT('',#21435);
#4888=VERTEX_POINT('',#21439);
#4889=VERTEX_POINT('',#21441);
#4890=VERTEX_POINT('',#21445);
#4891=VERTEX_POINT('',#21447);
#4892=VERTEX_POINT('',#21451);
#4893=VERTEX_POINT('',#21453);
#4894=VERTEX_POINT('',#21457);
#4895=VERTEX_POINT('',#21459);
#4896=VERTEX_POINT('',#21463);
#4897=VERTEX_POINT('',#21465);
#4898=VERTEX_POINT('',#21469);
#4899=VERTEX_POINT('',#21471);
#4900=VERTEX_POINT('',#21475);
#4901=VERTEX_POINT('',#21477);
#4902=VERTEX_POINT('',#21481);
#4903=VERTEX_POINT('',#21483);
#4904=VERTEX_POINT('',#21487);
#4905=VERTEX_POINT('',#21489);
#4906=VERTEX_POINT('',#21493);
#4907=VERTEX_POINT('',#21495);
#4908=VERTEX_POINT('',#21499);
#4909=VERTEX_POINT('',#21501);
#4910=VERTEX_POINT('',#21505);
#4911=VERTEX_POINT('',#21507);
#4912=VERTEX_POINT('',#21511);
#4913=VERTEX_POINT('',#21513);
#4914=VERTEX_POINT('',#21517);
#4915=VERTEX_POINT('',#21519);
#4916=VERTEX_POINT('',#21523);
#4917=VERTEX_POINT('',#21524);
#4918=VERTEX_POINT('',#21526);
#4919=VERTEX_POINT('',#21528);
#4920=VERTEX_POINT('',#21532);
#4921=VERTEX_POINT('',#21534);
#4922=VERTEX_POINT('',#21538);
#4923=VERTEX_POINT('',#21540);
#4924=VERTEX_POINT('',#21550);
#4925=VERTEX_POINT('',#21551);
#4926=VERTEX_POINT('',#21555);
#4927=VERTEX_POINT('',#21557);
#4928=VERTEX_POINT('',#21559);
#4929=VERTEX_POINT('',#21562);
#4930=VERTEX_POINT('',#21566);
#4931=VERTEX_POINT('',#21567);
#4932=VERTEX_POINT('',#21571);
#4933=VERTEX_POINT('',#21573);
#4934=VERTEX_POINT('',#21575);
#4935=VERTEX_POINT('',#21578);
#4936=VERTEX_POINT('',#21582);
#4937=VERTEX_POINT('',#21583);
#4938=VERTEX_POINT('',#21585);
#4939=VERTEX_POINT('',#21589);
#4940=VERTEX_POINT('',#21591);
#4941=VERTEX_POINT('',#21594);
#4942=VERTEX_POINT('',#21598);
#4943=VERTEX_POINT('',#21599);
#4944=VERTEX_POINT('',#21601);
#4945=VERTEX_POINT('',#21605);
#4946=VERTEX_POINT('',#21607);
#4947=VERTEX_POINT('',#21610);
#4948=VERTEX_POINT('',#21614);
#4949=VERTEX_POINT('',#21616);
#4950=VERTEX_POINT('',#21624);
#4951=VERTEX_POINT('',#21626);
#4952=VERTEX_POINT('',#21630);
#4953=VERTEX_POINT('',#21633);
#4954=VERTEX_POINT('',#21636);
#4955=VERTEX_POINT('',#21640);
#4956=VERTEX_POINT('',#21647);
#4957=VERTEX_POINT('',#21648);
#4958=VERTEX_POINT('',#21652);
#4959=VERTEX_POINT('',#21654);
#4960=VERTEX_POINT('',#21656);
#4961=VERTEX_POINT('',#21659);
#4962=VERTEX_POINT('',#21663);
#4963=VERTEX_POINT('',#21664);
#4964=VERTEX_POINT('',#21668);
#4965=VERTEX_POINT('',#21670);
#4966=VERTEX_POINT('',#21672);
#4967=VERTEX_POINT('',#21675);
#4968=VERTEX_POINT('',#21679);
#4969=VERTEX_POINT('',#21680);
#4970=VERTEX_POINT('',#21682);
#4971=VERTEX_POINT('',#21686);
#4972=VERTEX_POINT('',#21688);
#4973=VERTEX_POINT('',#21691);
#4974=VERTEX_POINT('',#21695);
#4975=VERTEX_POINT('',#21696);
#4976=VERTEX_POINT('',#21698);
#4977=VERTEX_POINT('',#21702);
#4978=VERTEX_POINT('',#21704);
#4979=VERTEX_POINT('',#21707);
#4980=VERTEX_POINT('',#21711);
#4981=VERTEX_POINT('',#21713);
#4982=VERTEX_POINT('',#21721);
#4983=VERTEX_POINT('',#21723);
#4984=VERTEX_POINT('',#21727);
#4985=VERTEX_POINT('',#21730);
#4986=VERTEX_POINT('',#21733);
#4987=VERTEX_POINT('',#21737);
#4988=VERTEX_POINT('',#21744);
#4989=VERTEX_POINT('',#21745);
#4990=VERTEX_POINT('',#21749);
#4991=VERTEX_POINT('',#21751);
#4992=VERTEX_POINT('',#21753);
#4993=VERTEX_POINT('',#21756);
#4994=VERTEX_POINT('',#21760);
#4995=VERTEX_POINT('',#21761);
#4996=VERTEX_POINT('',#21765);
#4997=VERTEX_POINT('',#21767);
#4998=VERTEX_POINT('',#21769);
#4999=VERTEX_POINT('',#21772);
#5000=VERTEX_POINT('',#21776);
#5001=VERTEX_POINT('',#21777);
#5002=VERTEX_POINT('',#21779);
#5003=VERTEX_POINT('',#21783);
#5004=VERTEX_POINT('',#21785);
#5005=VERTEX_POINT('',#21788);
#5006=VERTEX_POINT('',#21792);
#5007=VERTEX_POINT('',#21793);
#5008=VERTEX_POINT('',#21795);
#5009=VERTEX_POINT('',#21799);
#5010=VERTEX_POINT('',#21801);
#5011=VERTEX_POINT('',#21804);
#5012=VERTEX_POINT('',#21808);
#5013=VERTEX_POINT('',#21810);
#5014=VERTEX_POINT('',#21818);
#5015=VERTEX_POINT('',#21820);
#5016=VERTEX_POINT('',#21824);
#5017=VERTEX_POINT('',#21827);
#5018=VERTEX_POINT('',#21830);
#5019=VERTEX_POINT('',#21834);
#5020=VERTEX_POINT('',#21841);
#5021=VERTEX_POINT('',#21842);
#5022=VERTEX_POINT('',#21846);
#5023=VERTEX_POINT('',#21848);
#5024=VERTEX_POINT('',#21850);
#5025=VERTEX_POINT('',#21853);
#5026=VERTEX_POINT('',#21857);
#5027=VERTEX_POINT('',#21858);
#5028=VERTEX_POINT('',#21862);
#5029=VERTEX_POINT('',#21864);
#5030=VERTEX_POINT('',#21866);
#5031=VERTEX_POINT('',#21869);
#5032=VERTEX_POINT('',#21873);
#5033=VERTEX_POINT('',#21874);
#5034=VERTEX_POINT('',#21876);
#5035=VERTEX_POINT('',#21880);
#5036=VERTEX_POINT('',#21882);
#5037=VERTEX_POINT('',#21885);
#5038=VERTEX_POINT('',#21889);
#5039=VERTEX_POINT('',#21890);
#5040=VERTEX_POINT('',#21892);
#5041=VERTEX_POINT('',#21896);
#5042=VERTEX_POINT('',#21898);
#5043=VERTEX_POINT('',#21901);
#5044=VERTEX_POINT('',#21905);
#5045=VERTEX_POINT('',#21907);
#5046=VERTEX_POINT('',#21915);
#5047=VERTEX_POINT('',#21917);
#5048=VERTEX_POINT('',#21921);
#5049=VERTEX_POINT('',#21924);
#5050=VERTEX_POINT('',#21927);
#5051=VERTEX_POINT('',#21931);
#5052=VERTEX_POINT('',#21938);
#5053=VERTEX_POINT('',#21940);
#5054=VERTEX_POINT('',#21944);
#5055=VERTEX_POINT('',#21946);
#5056=VERTEX_POINT('',#21950);
#5057=VERTEX_POINT('',#21952);
#5058=VERTEX_POINT('',#21956);
#5059=VERTEX_POINT('',#21958);
#5060=VERTEX_POINT('',#21962);
#5061=VERTEX_POINT('',#21964);
#5062=VERTEX_POINT('',#21967);
#5063=VERTEX_POINT('',#21971);
#5064=VERTEX_POINT('',#21979);
#5065=VERTEX_POINT('',#21980);
#5066=VERTEX_POINT('',#21982);
#5067=VERTEX_POINT('',#21984);
#5068=VERTEX_POINT('',#21988);
#5069=VERTEX_POINT('',#21990);
#5070=VERTEX_POINT('',#21994);
#5071=VERTEX_POINT('',#21996);
#5072=VERTEX_POINT('',#22004);
#5073=VERTEX_POINT('',#22006);
#5074=VERTEX_POINT('',#22009);
#5075=VERTEX_POINT('',#22013);
#5076=VERTEX_POINT('',#22016);
#5077=VERTEX_POINT('',#22020);
#5078=VERTEX_POINT('',#22023);
#5079=VERTEX_POINT('',#22027);
#5080=VERTEX_POINT('',#22030);
#5081=VERTEX_POINT('',#22034);
#5082=VERTEX_POINT('',#22037);
#5083=VERTEX_POINT('',#22041);
#5084=VERTEX_POINT('',#22047);
#5085=VERTEX_POINT('',#22048);
#5086=VERTEX_POINT('',#22050);
#5087=VERTEX_POINT('',#22052);
#5088=VERTEX_POINT('',#22056);
#5089=VERTEX_POINT('',#22058);
#5090=VERTEX_POINT('',#22062);
#5091=VERTEX_POINT('',#22064);
#5092=VERTEX_POINT('',#22071);
#5093=VERTEX_POINT('',#22073);
#5094=VERTEX_POINT('',#22076);
#5095=VERTEX_POINT('',#22080);
#5096=VERTEX_POINT('',#22088);
#5097=VERTEX_POINT('',#22091);
#5098=VERTEX_POINT('',#22095);
#5099=VERTEX_POINT('',#22099);
#5100=VERTEX_POINT('',#22103);
#5101=VERTEX_POINT('',#22106);
#5102=VERTEX_POINT('',#22110);
#5103=VERTEX_POINT('',#22114);
#5104=VERTEX_POINT('',#22119);
#5105=VERTEX_POINT('',#22120);
#5106=VERTEX_POINT('',#22122);
#5107=VERTEX_POINT('',#22124);
#5108=VERTEX_POINT('',#22128);
#5109=VERTEX_POINT('',#22130);
#5110=VERTEX_POINT('',#22134);
#5111=VERTEX_POINT('',#22136);
#5112=VERTEX_POINT('',#22140);
#5113=VERTEX_POINT('',#22142);
#5114=VERTEX_POINT('',#22146);
#5115=VERTEX_POINT('',#22148);
#5116=EDGE_CURVE('',#4367,#4367,#3860,.T.);
#5117=EDGE_CURVE('',#4367,#4368,#2622,.T.);
#5118=EDGE_CURVE('',#4368,#4368,#3861,.T.);
#5119=EDGE_CURVE('',#4369,#4369,#3862,.T.);
#5120=EDGE_CURVE('',#4369,#4370,#2623,.T.);
#5121=EDGE_CURVE('',#4370,#4370,#3863,.T.);
#5122=EDGE_CURVE('',#4371,#4371,#3864,.T.);
#5123=EDGE_CURVE('',#4371,#4372,#2624,.T.);
#5124=EDGE_CURVE('',#4372,#4372,#3865,.T.);
#5125=EDGE_CURVE('',#4373,#4373,#3866,.T.);
#5126=EDGE_CURVE('',#4373,#4374,#2625,.T.);
#5127=EDGE_CURVE('',#4374,#4374,#3867,.T.);
#5128=EDGE_CURVE('',#4375,#4375,#3868,.T.);
#5129=EDGE_CURVE('',#4375,#4376,#2626,.T.);
#5130=EDGE_CURVE('',#4376,#4376,#3869,.T.);
#5131=EDGE_CURVE('',#4377,#4377,#3870,.T.);
#5132=EDGE_CURVE('',#4377,#4378,#2627,.T.);
#5133=EDGE_CURVE('',#4378,#4378,#3871,.T.);
#5134=EDGE_CURVE('',#4379,#4379,#3872,.T.);
#5135=EDGE_CURVE('',#4379,#4380,#2628,.T.);
#5136=EDGE_CURVE('',#4380,#4380,#3873,.T.);
#5137=EDGE_CURVE('',#4381,#4381,#3874,.T.);
#5138=EDGE_CURVE('',#4381,#4382,#2629,.T.);
#5139=EDGE_CURVE('',#4382,#4382,#3875,.T.);
#5140=EDGE_CURVE('',#4383,#4383,#3876,.T.);
#5141=EDGE_CURVE('',#4383,#4384,#2630,.T.);
#5142=EDGE_CURVE('',#4384,#4384,#3877,.T.);
#5143=EDGE_CURVE('',#4385,#4385,#3878,.T.);
#5144=EDGE_CURVE('',#4385,#4386,#2631,.T.);
#5145=EDGE_CURVE('',#4386,#4386,#3879,.T.);
#5146=EDGE_CURVE('',#4387,#4387,#3880,.T.);
#5147=EDGE_CURVE('',#4387,#4388,#2632,.T.);
#5148=EDGE_CURVE('',#4388,#4388,#3881,.T.);
#5149=EDGE_CURVE('',#4389,#4389,#3882,.T.);
#5150=EDGE_CURVE('',#4389,#4390,#2633,.T.);
#5151=EDGE_CURVE('',#4390,#4390,#3883,.T.);
#5152=EDGE_CURVE('',#4391,#4391,#3884,.T.);
#5153=EDGE_CURVE('',#4391,#4392,#2634,.T.);
#5154=EDGE_CURVE('',#4392,#4392,#3885,.T.);
#5155=EDGE_CURVE('',#4393,#4393,#3886,.T.);
#5156=EDGE_CURVE('',#4393,#4394,#2635,.T.);
#5157=EDGE_CURVE('',#4394,#4394,#3887,.T.);
#5158=EDGE_CURVE('',#4395,#4395,#3888,.T.);
#5159=EDGE_CURVE('',#4395,#4396,#2636,.T.);
#5160=EDGE_CURVE('',#4396,#4396,#3889,.T.);
#5161=EDGE_CURVE('',#4397,#4397,#3890,.T.);
#5162=EDGE_CURVE('',#4397,#4398,#2637,.T.);
#5163=EDGE_CURVE('',#4398,#4398,#3891,.T.);
#5164=EDGE_CURVE('',#4399,#4399,#3892,.T.);
#5165=EDGE_CURVE('',#4399,#4400,#2638,.T.);
#5166=EDGE_CURVE('',#4400,#4400,#3893,.T.);
#5167=EDGE_CURVE('',#4401,#4401,#3894,.T.);
#5168=EDGE_CURVE('',#4401,#4402,#2639,.T.);
#5169=EDGE_CURVE('',#4402,#4402,#3895,.T.);
#5170=EDGE_CURVE('',#4403,#4403,#3896,.T.);
#5171=EDGE_CURVE('',#4403,#4404,#2640,.T.);
#5172=EDGE_CURVE('',#4404,#4404,#3897,.T.);
#5173=EDGE_CURVE('',#4405,#4405,#3898,.T.);
#5174=EDGE_CURVE('',#4405,#4406,#2641,.T.);
#5175=EDGE_CURVE('',#4406,#4406,#3899,.T.);
#5176=EDGE_CURVE('',#4407,#4407,#3900,.T.);
#5177=EDGE_CURVE('',#4407,#4408,#2642,.T.);
#5178=EDGE_CURVE('',#4408,#4408,#3901,.T.);
#5179=EDGE_CURVE('',#4409,#4409,#3902,.T.);
#5180=EDGE_CURVE('',#4409,#4410,#2643,.T.);
#5181=EDGE_CURVE('',#4410,#4410,#3903,.T.);
#5182=EDGE_CURVE('',#4411,#4412,#2644,.T.);
#5183=EDGE_CURVE('',#4412,#4413,#2645,.T.);
#5184=EDGE_CURVE('',#4414,#4413,#2646,.T.);
#5185=EDGE_CURVE('',#4411,#4414,#2647,.T.);
#5186=EDGE_CURVE('',#4415,#4411,#2648,.T.);
#5187=EDGE_CURVE('',#4416,#4414,#2649,.T.);
#5188=EDGE_CURVE('',#4415,#4416,#2650,.T.);
#5189=EDGE_CURVE('',#4417,#4415,#2651,.T.);
#5190=EDGE_CURVE('',#4418,#4416,#2652,.T.);
#5191=EDGE_CURVE('',#4417,#4418,#2653,.T.);
#5192=EDGE_CURVE('',#4412,#4417,#2654,.T.);
#5193=EDGE_CURVE('',#4413,#4418,#2655,.T.);
#5194=EDGE_CURVE('',#4419,#4420,#2656,.T.);
#5195=EDGE_CURVE('',#4420,#4421,#2657,.T.);
#5196=EDGE_CURVE('',#4422,#4421,#2658,.T.);
#5197=EDGE_CURVE('',#4419,#4422,#2659,.T.);
#5198=EDGE_CURVE('',#4423,#4419,#2660,.T.);
#5199=EDGE_CURVE('',#4424,#4422,#2661,.T.);
#5200=EDGE_CURVE('',#4423,#4424,#2662,.T.);
#5201=EDGE_CURVE('',#4425,#4423,#2663,.T.);
#5202=EDGE_CURVE('',#4426,#4424,#2664,.T.);
#5203=EDGE_CURVE('',#4425,#4426,#2665,.T.);
#5204=EDGE_CURVE('',#4420,#4425,#2666,.T.);
#5205=EDGE_CURVE('',#4421,#4426,#2667,.T.);
#5206=EDGE_CURVE('',#4427,#4428,#2668,.T.);
#5207=EDGE_CURVE('',#4428,#4429,#2669,.T.);
#5208=EDGE_CURVE('',#4430,#4429,#2670,.T.);
#5209=EDGE_CURVE('',#4427,#4430,#2671,.T.);
#5210=EDGE_CURVE('',#4431,#4427,#2672,.T.);
#5211=EDGE_CURVE('',#4432,#4430,#2673,.T.);
#5212=EDGE_CURVE('',#4431,#4432,#2674,.T.);
#5213=EDGE_CURVE('',#4433,#4431,#2675,.T.);
#5214=EDGE_CURVE('',#4434,#4432,#2676,.T.);
#5215=EDGE_CURVE('',#4433,#4434,#2677,.T.);
#5216=EDGE_CURVE('',#4428,#4433,#2678,.T.);
#5217=EDGE_CURVE('',#4429,#4434,#2679,.T.);
#5218=EDGE_CURVE('',#4435,#4435,#3904,.T.);
#5219=EDGE_CURVE('',#4435,#4436,#2680,.T.);
#5220=EDGE_CURVE('',#4436,#4436,#3905,.T.);
#5221=EDGE_CURVE('',#4437,#4437,#3906,.T.);
#5222=EDGE_CURVE('',#4437,#4438,#2681,.T.);
#5223=EDGE_CURVE('',#4438,#4438,#3907,.T.);
#5224=EDGE_CURVE('',#4439,#4439,#3908,.T.);
#5225=EDGE_CURVE('',#4439,#4440,#2682,.T.);
#5226=EDGE_CURVE('',#4440,#4440,#3909,.T.);
#5227=EDGE_CURVE('',#4441,#4441,#3910,.T.);
#5228=EDGE_CURVE('',#4441,#4442,#2683,.T.);
#5229=EDGE_CURVE('',#4442,#4442,#3911,.T.);
#5230=EDGE_CURVE('',#4443,#4443,#3912,.T.);
#5231=EDGE_CURVE('',#4443,#4444,#2684,.T.);
#5232=EDGE_CURVE('',#4444,#4444,#3913,.T.);
#5233=EDGE_CURVE('',#4445,#4445,#3914,.T.);
#5234=EDGE_CURVE('',#4445,#4446,#2685,.T.);
#5235=EDGE_CURVE('',#4446,#4446,#3915,.T.);
#5236=EDGE_CURVE('',#4447,#4447,#3916,.T.);
#5237=EDGE_CURVE('',#4447,#4448,#2686,.T.);
#5238=EDGE_CURVE('',#4448,#4448,#3917,.T.);
#5239=EDGE_CURVE('',#4449,#4449,#3918,.T.);
#5240=EDGE_CURVE('',#4449,#4450,#2687,.T.);
#5241=EDGE_CURVE('',#4450,#4450,#3919,.T.);
#5242=EDGE_CURVE('',#4451,#4451,#3920,.T.);
#5243=EDGE_CURVE('',#4451,#4452,#2688,.T.);
#5244=EDGE_CURVE('',#4452,#4452,#3921,.T.);
#5245=EDGE_CURVE('',#4453,#4453,#3922,.T.);
#5246=EDGE_CURVE('',#4453,#4454,#2689,.T.);
#5247=EDGE_CURVE('',#4454,#4454,#3923,.T.);
#5248=EDGE_CURVE('',#4455,#4455,#3924,.T.);
#5249=EDGE_CURVE('',#4455,#4456,#2690,.T.);
#5250=EDGE_CURVE('',#4456,#4456,#3925,.T.);
#5251=EDGE_CURVE('',#4457,#4457,#3926,.T.);
#5252=EDGE_CURVE('',#4457,#4458,#2691,.T.);
#5253=EDGE_CURVE('',#4458,#4458,#3927,.T.);
#5254=EDGE_CURVE('',#4459,#4459,#3928,.T.);
#5255=EDGE_CURVE('',#4459,#4460,#2692,.T.);
#5256=EDGE_CURVE('',#4460,#4460,#3929,.T.);
#5257=EDGE_CURVE('',#4461,#4461,#3930,.T.);
#5258=EDGE_CURVE('',#4461,#4462,#2693,.T.);
#5259=EDGE_CURVE('',#4462,#4462,#3931,.T.);
#5260=EDGE_CURVE('',#4463,#4463,#3932,.T.);
#5261=EDGE_CURVE('',#4463,#4464,#2694,.T.);
#5262=EDGE_CURVE('',#4464,#4464,#3933,.T.);
#5263=EDGE_CURVE('',#4465,#4465,#3934,.T.);
#5264=EDGE_CURVE('',#4465,#4466,#2695,.T.);
#5265=EDGE_CURVE('',#4466,#4466,#3935,.T.);
#5266=EDGE_CURVE('',#4467,#4467,#3936,.T.);
#5267=EDGE_CURVE('',#4467,#4468,#2696,.T.);
#5268=EDGE_CURVE('',#4468,#4468,#3937,.T.);
#5269=EDGE_CURVE('',#4469,#4469,#3938,.T.);
#5270=EDGE_CURVE('',#4469,#4470,#2697,.T.);
#5271=EDGE_CURVE('',#4470,#4470,#3939,.T.);
#5272=EDGE_CURVE('',#4471,#4472,#2698,.T.);
#5273=EDGE_CURVE('',#4472,#4473,#2699,.T.);
#5274=EDGE_CURVE('',#4474,#4473,#2700,.T.);
#5275=EDGE_CURVE('',#4471,#4474,#2701,.T.);
#5276=EDGE_CURVE('',#4475,#4471,#2702,.T.);
#5277=EDGE_CURVE('',#4476,#4474,#2703,.T.);
#5278=EDGE_CURVE('',#4475,#4476,#2704,.T.);
#5279=EDGE_CURVE('',#4477,#4475,#2705,.T.);
#5280=EDGE_CURVE('',#4478,#4476,#2706,.T.);
#5281=EDGE_CURVE('',#4477,#4478,#2707,.T.);
#5282=EDGE_CURVE('',#4472,#4477,#2708,.T.);
#5283=EDGE_CURVE('',#4473,#4478,#2709,.T.);
#5284=EDGE_CURVE('',#4479,#4479,#3940,.T.);
#5285=EDGE_CURVE('',#4479,#4480,#2710,.T.);
#5286=EDGE_CURVE('',#4480,#4480,#3941,.T.);
#5287=EDGE_CURVE('',#4481,#4481,#3942,.T.);
#5288=EDGE_CURVE('',#4481,#4482,#2711,.T.);
#5289=EDGE_CURVE('',#4482,#4482,#3943,.T.);
#5290=EDGE_CURVE('',#4483,#4483,#3944,.T.);
#5291=EDGE_CURVE('',#4483,#4484,#2712,.T.);
#5292=EDGE_CURVE('',#4484,#4484,#3945,.T.);
#5293=EDGE_CURVE('',#4485,#4485,#3946,.T.);
#5294=EDGE_CURVE('',#4485,#4486,#2713,.T.);
#5295=EDGE_CURVE('',#4486,#4486,#3947,.T.);
#5296=EDGE_CURVE('',#4487,#4488,#2714,.T.);
#5297=EDGE_CURVE('',#4488,#4489,#2715,.T.);
#5298=EDGE_CURVE('',#4490,#4489,#2716,.T.);
#5299=EDGE_CURVE('',#4487,#4490,#2717,.T.);
#5300=EDGE_CURVE('',#4491,#4487,#2718,.T.);
#5301=EDGE_CURVE('',#4492,#4490,#2719,.T.);
#5302=EDGE_CURVE('',#4491,#4492,#2720,.T.);
#5303=EDGE_CURVE('',#4493,#4491,#2721,.T.);
#5304=EDGE_CURVE('',#4494,#4492,#2722,.T.);
#5305=EDGE_CURVE('',#4493,#4494,#2723,.T.);
#5306=EDGE_CURVE('',#4488,#4493,#2724,.T.);
#5307=EDGE_CURVE('',#4489,#4494,#2725,.T.);
#5308=EDGE_CURVE('',#4495,#4495,#3948,.T.);
#5309=EDGE_CURVE('',#4495,#4496,#2726,.T.);
#5310=EDGE_CURVE('',#4496,#4496,#3949,.T.);
#5311=EDGE_CURVE('',#4497,#4497,#3950,.T.);
#5312=EDGE_CURVE('',#4497,#4498,#2727,.T.);
#5313=EDGE_CURVE('',#4498,#4498,#3951,.T.);
#5314=EDGE_CURVE('',#4499,#4499,#3952,.T.);
#5315=EDGE_CURVE('',#4499,#4500,#2728,.T.);
#5316=EDGE_CURVE('',#4500,#4500,#3953,.T.);
#5317=EDGE_CURVE('',#4501,#4501,#3954,.T.);
#5318=EDGE_CURVE('',#4501,#4502,#2729,.T.);
#5319=EDGE_CURVE('',#4502,#4502,#3955,.T.);
#5320=EDGE_CURVE('',#4503,#4504,#2730,.T.);
#5321=EDGE_CURVE('',#4504,#4505,#2731,.T.);
#5322=EDGE_CURVE('',#4506,#4505,#2732,.T.);
#5323=EDGE_CURVE('',#4503,#4506,#2733,.T.);
#5324=EDGE_CURVE('',#4507,#4503,#2734,.T.);
#5325=EDGE_CURVE('',#4508,#4506,#2735,.T.);
#5326=EDGE_CURVE('',#4507,#4508,#2736,.T.);
#5327=EDGE_CURVE('',#4509,#4507,#2737,.T.);
#5328=EDGE_CURVE('',#4510,#4508,#2738,.T.);
#5329=EDGE_CURVE('',#4509,#4510,#2739,.T.);
#5330=EDGE_CURVE('',#4504,#4509,#2740,.T.);
#5331=EDGE_CURVE('',#4505,#4510,#2741,.T.);
#5332=EDGE_CURVE('',#4511,#4511,#3956,.T.);
#5333=EDGE_CURVE('',#4511,#4512,#2742,.T.);
#5334=EDGE_CURVE('',#4512,#4512,#3957,.T.);
#5335=EDGE_CURVE('',#4513,#4513,#3958,.T.);
#5336=EDGE_CURVE('',#4513,#4514,#2743,.T.);
#5337=EDGE_CURVE('',#4514,#4514,#3959,.T.);
#5338=EDGE_CURVE('',#4515,#4515,#3960,.T.);
#5339=EDGE_CURVE('',#4515,#4516,#2744,.T.);
#5340=EDGE_CURVE('',#4516,#4516,#3961,.T.);
#5341=EDGE_CURVE('',#4517,#4517,#3962,.T.);
#5342=EDGE_CURVE('',#4517,#4518,#2745,.T.);
#5343=EDGE_CURVE('',#4518,#4518,#3963,.T.);
#5344=EDGE_CURVE('',#4519,#4520,#2746,.T.);
#5345=EDGE_CURVE('',#4520,#4521,#2747,.T.);
#5346=EDGE_CURVE('',#4522,#4521,#2748,.T.);
#5347=EDGE_CURVE('',#4519,#4522,#2749,.T.);
#5348=EDGE_CURVE('',#4523,#4519,#2750,.T.);
#5349=EDGE_CURVE('',#4524,#4522,#2751,.T.);
#5350=EDGE_CURVE('',#4523,#4524,#2752,.T.);
#5351=EDGE_CURVE('',#4525,#4523,#2753,.T.);
#5352=EDGE_CURVE('',#4526,#4524,#2754,.T.);
#5353=EDGE_CURVE('',#4525,#4526,#2755,.T.);
#5354=EDGE_CURVE('',#4520,#4525,#2756,.T.);
#5355=EDGE_CURVE('',#4521,#4526,#2757,.T.);
#5356=EDGE_CURVE('',#4527,#4527,#3964,.T.);
#5357=EDGE_CURVE('',#4527,#4528,#2758,.T.);
#5358=EDGE_CURVE('',#4528,#4528,#3965,.T.);
#5359=EDGE_CURVE('',#4529,#4529,#3966,.T.);
#5360=EDGE_CURVE('',#4529,#4530,#2759,.T.);
#5361=EDGE_CURVE('',#4530,#4530,#3967,.T.);
#5362=EDGE_CURVE('',#4531,#4531,#3968,.T.);
#5363=EDGE_CURVE('',#4531,#4532,#2760,.T.);
#5364=EDGE_CURVE('',#4532,#4533,#3969,.T.);
#5365=EDGE_CURVE('',#4534,#4533,#2761,.T.);
#5366=EDGE_CURVE('',#4535,#4534,#3970,.T.);
#5367=EDGE_CURVE('',#4536,#4535,#2762,.T.);
#5368=EDGE_CURVE('',#4536,#4532,#3971,.T.);
#5369=EDGE_CURVE('',#4533,#4536,#2763,.T.);
#5370=EDGE_CURVE('',#4537,#4537,#3972,.T.);
#5371=EDGE_CURVE('',#4537,#4538,#2764,.T.);
#5372=EDGE_CURVE('',#4538,#4539,#3973,.T.);
#5373=EDGE_CURVE('',#4540,#4539,#2765,.T.);
#5374=EDGE_CURVE('',#4541,#4540,#3974,.T.);
#5375=EDGE_CURVE('',#4542,#4541,#2766,.T.);
#5376=EDGE_CURVE('',#4542,#4538,#3975,.T.);
#5377=EDGE_CURVE('',#4539,#4542,#2767,.T.);
#5378=EDGE_CURVE('',#4534,#4541,#2768,.T.);
#5379=EDGE_CURVE('',#4540,#4543,#2769,.T.);
#5380=EDGE_CURVE('',#4544,#4543,#2770,.T.);
#5381=EDGE_CURVE('',#4544,#4545,#2771,.T.);
#5382=EDGE_CURVE('',#4545,#4546,#2772,.T.);
#5383=EDGE_CURVE('',#4546,#4535,#2773,.T.);
#5384=EDGE_CURVE('',#4546,#4547,#2774,.T.);
#5385=EDGE_CURVE('',#4548,#4547,#2775,.T.);
#5386=EDGE_CURVE('',#4543,#4548,#2776,.T.);
#5387=EDGE_CURVE('',#4549,#4550,#2777,.T.);
#5388=EDGE_CURVE('',#4550,#4548,#2778,.T.);
#5389=EDGE_CURVE('',#4547,#4549,#2779,.T.);
#5390=EDGE_CURVE('',#4551,#4552,#2780,.T.);
#5391=EDGE_CURVE('',#4551,#4544,#2781,.T.);
#5392=EDGE_CURVE('',#4552,#4550,#2782,.T.);
#5393=EDGE_CURVE('',#4553,#4554,#2783,.T.);
#5394=EDGE_CURVE('',#4553,#4551,#2784,.T.);
#5395=EDGE_CURVE('',#4554,#4552,#2785,.T.);
#5396=EDGE_CURVE('',#4545,#4553,#2786,.T.);
#5397=EDGE_CURVE('',#4554,#4549,#2787,.T.);
#5398=EDGE_CURVE('',#4555,#4555,#3976,.T.);
#5399=EDGE_CURVE('',#4555,#4556,#2788,.T.);
#5400=EDGE_CURVE('',#4556,#4556,#3977,.T.);
#5401=EDGE_CURVE('',#4557,#4557,#3978,.T.);
#5402=EDGE_CURVE('',#4557,#4558,#2789,.T.);
#5403=EDGE_CURVE('',#4558,#4558,#3979,.T.);
#5404=EDGE_CURVE('',#4559,#4559,#3980,.T.);
#5405=EDGE_CURVE('',#4559,#4560,#586,.T.);
#5406=EDGE_CURVE('',#4560,#4560,#3981,.T.);
#5407=EDGE_CURVE('',#4561,#4561,#3982,.T.);
#5408=EDGE_CURVE('',#4561,#4562,#2790,.T.);
#5409=EDGE_CURVE('',#4562,#4562,#3983,.T.);
#5410=EDGE_CURVE('',#4563,#4563,#3984,.T.);
#5411=EDGE_CURVE('',#4563,#4564,#2791,.T.);
#5412=EDGE_CURVE('',#4564,#4564,#3985,.T.);
#5413=EDGE_CURVE('',#4565,#4565,#3986,.T.);
#5414=EDGE_CURVE('',#4565,#4566,#2792,.T.);
#5415=EDGE_CURVE('',#4566,#4566,#3987,.T.);
#5416=EDGE_CURVE('',#4567,#4567,#3988,.T.);
#5417=EDGE_CURVE('',#4567,#4568,#2793,.T.);
#5418=EDGE_CURVE('',#4568,#4568,#3989,.T.);
#5419=EDGE_CURVE('',#4569,#4570,#2794,.T.);
#5420=EDGE_CURVE('',#4570,#4571,#2795,.T.);
#5421=EDGE_CURVE('',#4572,#4571,#2796,.T.);
#5422=EDGE_CURVE('',#4569,#4572,#2797,.T.);
#5423=EDGE_CURVE('',#4573,#4569,#2798,.T.);
#5424=EDGE_CURVE('',#4574,#4572,#2799,.T.);
#5425=EDGE_CURVE('',#4573,#4574,#2800,.T.);
#5426=EDGE_CURVE('',#4575,#4573,#2801,.T.);
#5427=EDGE_CURVE('',#4576,#4574,#2802,.T.);
#5428=EDGE_CURVE('',#4575,#4576,#2803,.T.);
#5429=EDGE_CURVE('',#4570,#4575,#2804,.T.);
#5430=EDGE_CURVE('',#4571,#4576,#2805,.T.);
#5431=EDGE_CURVE('',#4577,#4577,#3990,.T.);
#5432=EDGE_CURVE('',#4577,#4578,#2806,.T.);
#5433=EDGE_CURVE('',#4578,#4578,#3991,.T.);
#5434=EDGE_CURVE('',#4579,#4579,#3992,.T.);
#5435=EDGE_CURVE('',#4579,#4580,#2807,.T.);
#5436=EDGE_CURVE('',#4580,#4580,#3993,.T.);
#5437=EDGE_CURVE('',#4581,#4581,#3994,.T.);
#5438=EDGE_CURVE('',#4581,#4582,#2808,.T.);
#5439=EDGE_CURVE('',#4582,#4583,#3995,.T.);
#5440=EDGE_CURVE('',#4584,#4583,#2809,.T.);
#5441=EDGE_CURVE('',#4585,#4584,#3996,.T.);
#5442=EDGE_CURVE('',#4586,#4585,#2810,.T.);
#5443=EDGE_CURVE('',#4586,#4582,#3997,.T.);
#5444=EDGE_CURVE('',#4583,#4586,#2811,.T.);
#5445=EDGE_CURVE('',#4587,#4587,#3998,.T.);
#5446=EDGE_CURVE('',#4587,#4588,#2812,.T.);
#5447=EDGE_CURVE('',#4588,#4589,#3999,.T.);
#5448=EDGE_CURVE('',#4590,#4589,#2813,.T.);
#5449=EDGE_CURVE('',#4591,#4590,#4000,.T.);
#5450=EDGE_CURVE('',#4592,#4591,#2814,.T.);
#5451=EDGE_CURVE('',#4592,#4588,#4001,.T.);
#5452=EDGE_CURVE('',#4589,#4592,#2815,.T.);
#5453=EDGE_CURVE('',#4584,#4591,#2816,.T.);
#5454=EDGE_CURVE('',#4590,#4593,#2817,.T.);
#5455=EDGE_CURVE('',#4594,#4593,#2818,.T.);
#5456=EDGE_CURVE('',#4594,#4595,#2819,.T.);
#5457=EDGE_CURVE('',#4595,#4596,#2820,.T.);
#5458=EDGE_CURVE('',#4596,#4585,#2821,.T.);
#5459=EDGE_CURVE('',#4596,#4597,#2822,.T.);
#5460=EDGE_CURVE('',#4598,#4597,#2823,.T.);
#5461=EDGE_CURVE('',#4593,#4598,#2824,.T.);
#5462=EDGE_CURVE('',#4599,#4600,#2825,.T.);
#5463=EDGE_CURVE('',#4600,#4598,#2826,.T.);
#5464=EDGE_CURVE('',#4597,#4599,#2827,.T.);
#5465=EDGE_CURVE('',#4601,#4602,#2828,.T.);
#5466=EDGE_CURVE('',#4601,#4594,#2829,.T.);
#5467=EDGE_CURVE('',#4602,#4600,#2830,.T.);
#5468=EDGE_CURVE('',#4603,#4604,#2831,.T.);
#5469=EDGE_CURVE('',#4603,#4601,#2832,.T.);
#5470=EDGE_CURVE('',#4604,#4602,#2833,.T.);
#5471=EDGE_CURVE('',#4595,#4603,#2834,.T.);
#5472=EDGE_CURVE('',#4604,#4599,#2835,.T.);
#5473=EDGE_CURVE('',#4605,#4605,#4002,.T.);
#5474=EDGE_CURVE('',#4605,#4606,#2836,.T.);
#5475=EDGE_CURVE('',#4606,#4606,#4003,.T.);
#5476=EDGE_CURVE('',#4607,#4607,#4004,.T.);
#5477=EDGE_CURVE('',#4607,#4608,#2837,.T.);
#5478=EDGE_CURVE('',#4608,#4608,#4005,.T.);
#5479=EDGE_CURVE('',#4609,#4609,#4006,.T.);
#5480=EDGE_CURVE('',#4609,#4610,#587,.T.);
#5481=EDGE_CURVE('',#4610,#4610,#4007,.T.);
#5482=EDGE_CURVE('',#4611,#4611,#4008,.T.);
#5483=EDGE_CURVE('',#4611,#4612,#2838,.T.);
#5484=EDGE_CURVE('',#4612,#4612,#4009,.T.);
#5485=EDGE_CURVE('',#4613,#4613,#4010,.T.);
#5486=EDGE_CURVE('',#4613,#4614,#2839,.T.);
#5487=EDGE_CURVE('',#4614,#4614,#4011,.T.);
#5488=EDGE_CURVE('',#4615,#4615,#4012,.T.);
#5489=EDGE_CURVE('',#4615,#4616,#2840,.T.);
#5490=EDGE_CURVE('',#4616,#4616,#4013,.T.);
#5491=EDGE_CURVE('',#4617,#4617,#4014,.T.);
#5492=EDGE_CURVE('',#4617,#4618,#2841,.T.);
#5493=EDGE_CURVE('',#4618,#4618,#4015,.T.);
#5494=EDGE_CURVE('',#4619,#4620,#2842,.T.);
#5495=EDGE_CURVE('',#4620,#4621,#2843,.T.);
#5496=EDGE_CURVE('',#4622,#4621,#2844,.T.);
#5497=EDGE_CURVE('',#4619,#4622,#2845,.T.);
#5498=EDGE_CURVE('',#4623,#4619,#2846,.T.);
#5499=EDGE_CURVE('',#4624,#4622,#2847,.T.);
#5500=EDGE_CURVE('',#4623,#4624,#2848,.T.);
#5501=EDGE_CURVE('',#4625,#4623,#2849,.T.);
#5502=EDGE_CURVE('',#4626,#4624,#2850,.T.);
#5503=EDGE_CURVE('',#4625,#4626,#2851,.T.);
#5504=EDGE_CURVE('',#4620,#4625,#2852,.T.);
#5505=EDGE_CURVE('',#4621,#4626,#2853,.T.);
#5506=EDGE_CURVE('',#4627,#4627,#4016,.T.);
#5507=EDGE_CURVE('',#4627,#4628,#2854,.T.);
#5508=EDGE_CURVE('',#4628,#4628,#4017,.T.);
#5509=EDGE_CURVE('',#4629,#4629,#4018,.T.);
#5510=EDGE_CURVE('',#4629,#4630,#2855,.T.);
#5511=EDGE_CURVE('',#4630,#4630,#4019,.T.);
#5512=EDGE_CURVE('',#4631,#4631,#4020,.T.);
#5513=EDGE_CURVE('',#4631,#4632,#2856,.T.);
#5514=EDGE_CURVE('',#4632,#4633,#4021,.T.);
#5515=EDGE_CURVE('',#4634,#4633,#2857,.T.);
#5516=EDGE_CURVE('',#4635,#4634,#4022,.T.);
#5517=EDGE_CURVE('',#4636,#4635,#2858,.T.);
#5518=EDGE_CURVE('',#4636,#4632,#4023,.T.);
#5519=EDGE_CURVE('',#4633,#4636,#2859,.T.);
#5520=EDGE_CURVE('',#4637,#4637,#4024,.T.);
#5521=EDGE_CURVE('',#4637,#4638,#2860,.T.);
#5522=EDGE_CURVE('',#4638,#4639,#4025,.T.);
#5523=EDGE_CURVE('',#4640,#4639,#2861,.T.);
#5524=EDGE_CURVE('',#4641,#4640,#4026,.T.);
#5525=EDGE_CURVE('',#4642,#4641,#2862,.T.);
#5526=EDGE_CURVE('',#4642,#4638,#4027,.T.);
#5527=EDGE_CURVE('',#4639,#4642,#2863,.T.);
#5528=EDGE_CURVE('',#4634,#4641,#2864,.T.);
#5529=EDGE_CURVE('',#4640,#4643,#2865,.T.);
#5530=EDGE_CURVE('',#4644,#4643,#2866,.T.);
#5531=EDGE_CURVE('',#4644,#4645,#2867,.T.);
#5532=EDGE_CURVE('',#4645,#4646,#2868,.T.);
#5533=EDGE_CURVE('',#4646,#4635,#2869,.T.);
#5534=EDGE_CURVE('',#4646,#4647,#2870,.T.);
#5535=EDGE_CURVE('',#4648,#4647,#2871,.T.);
#5536=EDGE_CURVE('',#4643,#4648,#2872,.T.);
#5537=EDGE_CURVE('',#4649,#4650,#2873,.T.);
#5538=EDGE_CURVE('',#4650,#4648,#2874,.T.);
#5539=EDGE_CURVE('',#4647,#4649,#2875,.T.);
#5540=EDGE_CURVE('',#4651,#4652,#2876,.T.);
#5541=EDGE_CURVE('',#4651,#4644,#2877,.T.);
#5542=EDGE_CURVE('',#4652,#4650,#2878,.T.);
#5543=EDGE_CURVE('',#4653,#4654,#2879,.T.);
#5544=EDGE_CURVE('',#4653,#4651,#2880,.T.);
#5545=EDGE_CURVE('',#4654,#4652,#2881,.T.);
#5546=EDGE_CURVE('',#4645,#4653,#2882,.T.);
#5547=EDGE_CURVE('',#4654,#4649,#2883,.T.);
#5548=EDGE_CURVE('',#4655,#4655,#4028,.T.);
#5549=EDGE_CURVE('',#4655,#4656,#2884,.T.);
#5550=EDGE_CURVE('',#4656,#4656,#4029,.T.);
#5551=EDGE_CURVE('',#4657,#4657,#4030,.T.);
#5552=EDGE_CURVE('',#4657,#4658,#2885,.T.);
#5553=EDGE_CURVE('',#4658,#4658,#4031,.T.);
#5554=EDGE_CURVE('',#4659,#4659,#4032,.T.);
#5555=EDGE_CURVE('',#4659,#4660,#588,.T.);
#5556=EDGE_CURVE('',#4660,#4660,#4033,.T.);
#5557=EDGE_CURVE('',#4661,#4661,#4034,.T.);
#5558=EDGE_CURVE('',#4661,#4662,#2886,.T.);
#5559=EDGE_CURVE('',#4662,#4662,#4035,.T.);
#5560=EDGE_CURVE('',#4663,#4663,#4036,.T.);
#5561=EDGE_CURVE('',#4663,#4664,#2887,.T.);
#5562=EDGE_CURVE('',#4664,#4664,#4037,.T.);
#5563=EDGE_CURVE('',#4665,#4665,#4038,.T.);
#5564=EDGE_CURVE('',#4665,#4666,#2888,.T.);
#5565=EDGE_CURVE('',#4666,#4666,#4039,.T.);
#5566=EDGE_CURVE('',#4667,#4667,#4040,.T.);
#5567=EDGE_CURVE('',#4667,#4668,#2889,.T.);
#5568=EDGE_CURVE('',#4668,#4668,#4041,.T.);
#5569=EDGE_CURVE('',#4669,#4670,#2890,.T.);
#5570=EDGE_CURVE('',#4670,#4671,#2891,.T.);
#5571=EDGE_CURVE('',#4672,#4671,#2892,.T.);
#5572=EDGE_CURVE('',#4669,#4672,#2893,.T.);
#5573=EDGE_CURVE('',#4673,#4669,#2894,.T.);
#5574=EDGE_CURVE('',#4674,#4672,#2895,.T.);
#5575=EDGE_CURVE('',#4673,#4674,#2896,.T.);
#5576=EDGE_CURVE('',#4675,#4673,#2897,.T.);
#5577=EDGE_CURVE('',#4676,#4674,#2898,.T.);
#5578=EDGE_CURVE('',#4675,#4676,#2899,.T.);
#5579=EDGE_CURVE('',#4670,#4675,#2900,.T.);
#5580=EDGE_CURVE('',#4671,#4676,#2901,.T.);
#5581=EDGE_CURVE('',#4677,#4677,#4042,.T.);
#5582=EDGE_CURVE('',#4677,#4678,#2902,.T.);
#5583=EDGE_CURVE('',#4678,#4678,#4043,.T.);
#5584=EDGE_CURVE('',#4679,#4679,#4044,.T.);
#5585=EDGE_CURVE('',#4679,#4680,#2903,.T.);
#5586=EDGE_CURVE('',#4680,#4680,#4045,.T.);
#5587=EDGE_CURVE('',#4681,#4681,#4046,.T.);
#5588=EDGE_CURVE('',#4681,#4682,#2904,.T.);
#5589=EDGE_CURVE('',#4682,#4683,#4047,.T.);
#5590=EDGE_CURVE('',#4684,#4683,#2905,.T.);
#5591=EDGE_CURVE('',#4685,#4684,#4048,.T.);
#5592=EDGE_CURVE('',#4686,#4685,#2906,.T.);
#5593=EDGE_CURVE('',#4686,#4682,#4049,.T.);
#5594=EDGE_CURVE('',#4683,#4686,#2907,.T.);
#5595=EDGE_CURVE('',#4687,#4687,#4050,.T.);
#5596=EDGE_CURVE('',#4687,#4688,#2908,.T.);
#5597=EDGE_CURVE('',#4688,#4689,#4051,.T.);
#5598=EDGE_CURVE('',#4690,#4689,#2909,.T.);
#5599=EDGE_CURVE('',#4691,#4690,#4052,.T.);
#5600=EDGE_CURVE('',#4692,#4691,#2910,.T.);
#5601=EDGE_CURVE('',#4692,#4688,#4053,.T.);
#5602=EDGE_CURVE('',#4689,#4692,#2911,.T.);
#5603=EDGE_CURVE('',#4684,#4691,#2912,.T.);
#5604=EDGE_CURVE('',#4690,#4693,#2913,.T.);
#5605=EDGE_CURVE('',#4694,#4693,#2914,.T.);
#5606=EDGE_CURVE('',#4694,#4695,#2915,.T.);
#5607=EDGE_CURVE('',#4695,#4696,#2916,.T.);
#5608=EDGE_CURVE('',#4696,#4685,#2917,.T.);
#5609=EDGE_CURVE('',#4696,#4697,#2918,.T.);
#5610=EDGE_CURVE('',#4698,#4697,#2919,.T.);
#5611=EDGE_CURVE('',#4693,#4698,#2920,.T.);
#5612=EDGE_CURVE('',#4699,#4700,#2921,.T.);
#5613=EDGE_CURVE('',#4700,#4698,#2922,.T.);
#5614=EDGE_CURVE('',#4697,#4699,#2923,.T.);
#5615=EDGE_CURVE('',#4701,#4702,#2924,.T.);
#5616=EDGE_CURVE('',#4701,#4694,#2925,.T.);
#5617=EDGE_CURVE('',#4702,#4700,#2926,.T.);
#5618=EDGE_CURVE('',#4703,#4704,#2927,.T.);
#5619=EDGE_CURVE('',#4703,#4701,#2928,.T.);
#5620=EDGE_CURVE('',#4704,#4702,#2929,.T.);
#5621=EDGE_CURVE('',#4695,#4703,#2930,.T.);
#5622=EDGE_CURVE('',#4704,#4699,#2931,.T.);
#5623=EDGE_CURVE('',#4705,#4705,#4054,.T.);
#5624=EDGE_CURVE('',#4705,#4706,#2932,.T.);
#5625=EDGE_CURVE('',#4706,#4706,#4055,.T.);
#5626=EDGE_CURVE('',#4707,#4707,#4056,.T.);
#5627=EDGE_CURVE('',#4707,#4708,#2933,.T.);
#5628=EDGE_CURVE('',#4708,#4708,#4057,.T.);
#5629=EDGE_CURVE('',#4709,#4709,#4058,.T.);
#5630=EDGE_CURVE('',#4709,#4710,#589,.T.);
#5631=EDGE_CURVE('',#4710,#4710,#4059,.T.);
#5632=EDGE_CURVE('',#4711,#4711,#4060,.T.);
#5633=EDGE_CURVE('',#4711,#4712,#2934,.T.);
#5634=EDGE_CURVE('',#4712,#4712,#4061,.T.);
#5635=EDGE_CURVE('',#4713,#4713,#4062,.T.);
#5636=EDGE_CURVE('',#4713,#4714,#2935,.T.);
#5637=EDGE_CURVE('',#4714,#4714,#4063,.T.);
#5638=EDGE_CURVE('',#4715,#4715,#4064,.T.);
#5639=EDGE_CURVE('',#4715,#4716,#2936,.T.);
#5640=EDGE_CURVE('',#4716,#4716,#4065,.T.);
#5641=EDGE_CURVE('',#4717,#4717,#4066,.T.);
#5642=EDGE_CURVE('',#4717,#4718,#2937,.T.);
#5643=EDGE_CURVE('',#4718,#4718,#4067,.T.);
#5644=EDGE_CURVE('',#4719,#4719,#4068,.T.);
#5645=EDGE_CURVE('',#4719,#4720,#2938,.T.);
#5646=EDGE_CURVE('',#4720,#4720,#4069,.T.);
#5647=EDGE_CURVE('',#4721,#4721,#4070,.T.);
#5648=EDGE_CURVE('',#4721,#4722,#2939,.T.);
#5649=EDGE_CURVE('',#4722,#4722,#4071,.T.);
#5650=EDGE_CURVE('',#4723,#4724,#2940,.T.);
#5651=EDGE_CURVE('',#4724,#4725,#2941,.T.);
#5652=EDGE_CURVE('',#4726,#4725,#2942,.T.);
#5653=EDGE_CURVE('',#4723,#4726,#2943,.T.);
#5654=EDGE_CURVE('',#4727,#4723,#2944,.T.);
#5655=EDGE_CURVE('',#4728,#4726,#2945,.T.);
#5656=EDGE_CURVE('',#4727,#4728,#2946,.T.);
#5657=EDGE_CURVE('',#4729,#4727,#2947,.T.);
#5658=EDGE_CURVE('',#4730,#4728,#2948,.T.);
#5659=EDGE_CURVE('',#4729,#4730,#2949,.T.);
#5660=EDGE_CURVE('',#4724,#4729,#2950,.T.);
#5661=EDGE_CURVE('',#4725,#4730,#2951,.T.);
#5662=EDGE_CURVE('',#4731,#4731,#4072,.T.);
#5663=EDGE_CURVE('',#4731,#4732,#2952,.T.);
#5664=EDGE_CURVE('',#4732,#4732,#4073,.T.);
#5665=EDGE_CURVE('',#4733,#4733,#4074,.T.);
#5666=EDGE_CURVE('',#4733,#4734,#2953,.T.);
#5667=EDGE_CURVE('',#4734,#4734,#4075,.T.);
#5668=EDGE_CURVE('',#4735,#4735,#4076,.T.);
#5669=EDGE_CURVE('',#4735,#4736,#2954,.T.);
#5670=EDGE_CURVE('',#4736,#4736,#4077,.T.);
#5671=EDGE_CURVE('',#4737,#4737,#4078,.T.);
#5672=EDGE_CURVE('',#4737,#4738,#2955,.T.);
#5673=EDGE_CURVE('',#4738,#4738,#4079,.T.);
#5674=EDGE_CURVE('',#4739,#4739,#4080,.T.);
#5675=EDGE_CURVE('',#4739,#4740,#2956,.T.);
#5676=EDGE_CURVE('',#4740,#4740,#4081,.T.);
#5677=EDGE_CURVE('',#4741,#4741,#4082,.T.);
#5678=EDGE_CURVE('',#4741,#4742,#2957,.T.);
#5679=EDGE_CURVE('',#4742,#4742,#4083,.T.);
#5680=EDGE_CURVE('',#4743,#4743,#4084,.T.);
#5681=EDGE_CURVE('',#4743,#4744,#2958,.T.);
#5682=EDGE_CURVE('',#4744,#4744,#4085,.T.);
#5683=EDGE_CURVE('',#4745,#4745,#4086,.T.);
#5684=EDGE_CURVE('',#4745,#4746,#2959,.T.);
#5685=EDGE_CURVE('',#4746,#4746,#4087,.T.);
#5686=EDGE_CURVE('',#4747,#4748,#2960,.T.);
#5687=EDGE_CURVE('',#4748,#4749,#2961,.T.);
#5688=EDGE_CURVE('',#4750,#4749,#2962,.T.);
#5689=EDGE_CURVE('',#4747,#4750,#2963,.T.);
#5690=EDGE_CURVE('',#4751,#4747,#2964,.T.);
#5691=EDGE_CURVE('',#4752,#4750,#2965,.T.);
#5692=EDGE_CURVE('',#4751,#4752,#2966,.T.);
#5693=EDGE_CURVE('',#4753,#4751,#2967,.T.);
#5694=EDGE_CURVE('',#4754,#4752,#2968,.T.);
#5695=EDGE_CURVE('',#4753,#4754,#2969,.T.);
#5696=EDGE_CURVE('',#4748,#4753,#2970,.T.);
#5697=EDGE_CURVE('',#4749,#4754,#2971,.T.);
#5698=EDGE_CURVE('',#4755,#4755,#4088,.T.);
#5699=EDGE_CURVE('',#4755,#4756,#2972,.T.);
#5700=EDGE_CURVE('',#4756,#4756,#4089,.T.);
#5701=EDGE_CURVE('',#4757,#4757,#4090,.T.);
#5702=EDGE_CURVE('',#4757,#4758,#2973,.T.);
#5703=EDGE_CURVE('',#4758,#4758,#4091,.T.);
#5704=EDGE_CURVE('',#4759,#4759,#4092,.T.);
#5705=EDGE_CURVE('',#4759,#4760,#2974,.T.);
#5706=EDGE_CURVE('',#4760,#4760,#4093,.T.);
#5707=EDGE_CURVE('',#4761,#4761,#4094,.T.);
#5708=EDGE_CURVE('',#4761,#4762,#2975,.T.);
#5709=EDGE_CURVE('',#4762,#4762,#4095,.T.);
#5710=EDGE_CURVE('',#4763,#4763,#4096,.T.);
#5711=EDGE_CURVE('',#4763,#4764,#2976,.T.);
#5712=EDGE_CURVE('',#4764,#4764,#4097,.T.);
#5713=EDGE_CURVE('',#4765,#4765,#4098,.T.);
#5714=EDGE_CURVE('',#4765,#4766,#2977,.T.);
#5715=EDGE_CURVE('',#4766,#4766,#4099,.T.);
#5716=EDGE_CURVE('',#4767,#4767,#4100,.T.);
#5717=EDGE_CURVE('',#4767,#4768,#2978,.T.);
#5718=EDGE_CURVE('',#4768,#4768,#4101,.T.);
#5719=EDGE_CURVE('',#4769,#4769,#4102,.T.);
#5720=EDGE_CURVE('',#4769,#4770,#2979,.T.);
#5721=EDGE_CURVE('',#4770,#4770,#4103,.T.);
#5722=EDGE_CURVE('',#4771,#4771,#4104,.T.);
#5723=EDGE_CURVE('',#4771,#4772,#2980,.T.);
#5724=EDGE_CURVE('',#4772,#4772,#4105,.T.);
#5725=EDGE_CURVE('',#4773,#4773,#4106,.T.);
#5726=EDGE_CURVE('',#4773,#4774,#2981,.T.);
#5727=EDGE_CURVE('',#4774,#4774,#4107,.T.);
#5728=EDGE_CURVE('',#4775,#4775,#4108,.T.);
#5729=EDGE_CURVE('',#4775,#4776,#2982,.T.);
#5730=EDGE_CURVE('',#4776,#4776,#4109,.T.);
#5731=EDGE_CURVE('',#4777,#4777,#4110,.T.);
#5732=EDGE_CURVE('',#4777,#4778,#2983,.T.);
#5733=EDGE_CURVE('',#4778,#4778,#4111,.T.);
#5734=EDGE_CURVE('',#4779,#4779,#4112,.T.);
#5735=EDGE_CURVE('',#4779,#4780,#2984,.T.);
#5736=EDGE_CURVE('',#4780,#4780,#4113,.T.);
#5737=EDGE_CURVE('',#4781,#4781,#4114,.T.);
#5738=EDGE_CURVE('',#4781,#4782,#2985,.T.);
#5739=EDGE_CURVE('',#4782,#4782,#4115,.T.);
#5740=EDGE_CURVE('',#4783,#4783,#4116,.T.);
#5741=EDGE_CURVE('',#4783,#4784,#2986,.T.);
#5742=EDGE_CURVE('',#4784,#4784,#4117,.T.);
#5743=EDGE_CURVE('',#4785,#4785,#4118,.T.);
#5744=EDGE_CURVE('',#4785,#4783,#2987,.T.);
#5745=EDGE_CURVE('',#4786,#4786,#4119,.T.);
#5746=EDGE_CURVE('',#4786,#4785,#2988,.T.);
#5747=EDGE_CURVE('',#4787,#4788,#2989,.T.);
#5748=EDGE_CURVE('',#4788,#4787,#4120,.T.);
#5749=EDGE_CURVE('',#4789,#4787,#2990,.T.);
#5750=EDGE_CURVE('',#4790,#4789,#4121,.T.);
#5751=EDGE_CURVE('',#4788,#4790,#2991,.T.);
#5752=EDGE_CURVE('',#4791,#4792,#2992,.T.);
#5753=EDGE_CURVE('',#4791,#4793,#4122,.T.);
#5754=EDGE_CURVE('',#4794,#4793,#2993,.T.);
#5755=EDGE_CURVE('',#4792,#4794,#4123,.T.);
#5756=EDGE_CURVE('',#4793,#4791,#2994,.T.);
#5757=EDGE_CURVE('',#4789,#4795,#2995,.T.);
#5758=EDGE_CURVE('',#4796,#4795,#2996,.T.);
#5759=EDGE_CURVE('',#4796,#4797,#2997,.T.);
#5760=EDGE_CURVE('',#4798,#4797,#2998,.T.);
#5761=EDGE_CURVE('',#4798,#4790,#2999,.T.);
#5762=EDGE_CURVE('',#4799,#4799,#4124,.T.);
#5763=EDGE_CURVE('',#4800,#4798,#3000,.T.);
#5764=EDGE_CURVE('',#4800,#4801,#3001,.T.);
#5765=EDGE_CURVE('',#4795,#4801,#3002,.T.);
#5766=EDGE_CURVE('',#4802,#4802,#4125,.T.);
#5767=EDGE_CURVE('',#4803,#4804,#3003,.T.);
#5768=EDGE_CURVE('',#4805,#4804,#3004,.T.);
#5769=EDGE_CURVE('',#4792,#4805,#3005,.T.);
#5770=EDGE_CURVE('',#4806,#4794,#3006,.T.);
#5771=EDGE_CURVE('',#4803,#4806,#3007,.T.);
#5772=EDGE_CURVE('',#4807,#4807,#4126,.T.);
#5773=EDGE_CURVE('',#4808,#4808,#4127,.T.);
#5774=EDGE_CURVE('',#4808,#4809,#3008,.T.);
#5775=EDGE_CURVE('',#4809,#4809,#4128,.T.);
#5776=EDGE_CURVE('',#4802,#4810,#3009,.T.);
#5777=EDGE_CURVE('',#4810,#4810,#4129,.T.);
#5778=EDGE_CURVE('',#4811,#4811,#4130,.T.);
#5779=EDGE_CURVE('',#4811,#4799,#3010,.T.);
#5780=EDGE_CURVE('',#4812,#4812,#4131,.T.);
#5781=EDGE_CURVE('',#4812,#4807,#3011,.T.);
#5782=EDGE_CURVE('',#4813,#4813,#4132,.T.);
#5783=EDGE_CURVE('',#4813,#4814,#3012,.T.);
#5784=EDGE_CURVE('',#4814,#4814,#4133,.T.);
#5785=EDGE_CURVE('',#4797,#4815,#3013,.T.);
#5786=EDGE_CURVE('',#4815,#4816,#3014,.T.);
#5787=EDGE_CURVE('',#4816,#4803,#3015,.T.);
#5788=EDGE_CURVE('',#4806,#4817,#3016,.T.);
#5789=EDGE_CURVE('',#4817,#4818,#3017,.T.);
#5790=EDGE_CURVE('',#4818,#4819,#3018,.T.);
#5791=EDGE_CURVE('',#4819,#4820,#3019,.T.);
#5792=EDGE_CURVE('',#4820,#4821,#3020,.T.);
#5793=EDGE_CURVE('',#4821,#4800,#3021,.T.);
#5794=EDGE_CURVE('',#4822,#4796,#3022,.T.);
#5795=EDGE_CURVE('',#4815,#4822,#3023,.T.);
#5796=EDGE_CURVE('',#4823,#4822,#3024,.T.);
#5797=EDGE_CURVE('',#4816,#4823,#3025,.T.);
#5798=EDGE_CURVE('',#4804,#4823,#3026,.T.);
#5799=EDGE_CURVE('',#4824,#4805,#3027,.T.);
#5800=EDGE_CURVE('',#4817,#4824,#3028,.T.);
#5801=EDGE_CURVE('',#4825,#4824,#3029,.T.);
#5802=EDGE_CURVE('',#4818,#4825,#3030,.T.);
#5803=EDGE_CURVE('',#4826,#4825,#3031,.T.);
#5804=EDGE_CURVE('',#4819,#4826,#3032,.T.);
#5805=EDGE_CURVE('',#4827,#4826,#3033,.T.);
#5806=EDGE_CURVE('',#4820,#4827,#3034,.T.);
#5807=EDGE_CURVE('',#4828,#4827,#3035,.T.);
#5808=EDGE_CURVE('',#4821,#4828,#3036,.T.);
#5809=EDGE_CURVE('',#4801,#4828,#3037,.T.);
#5810=EDGE_CURVE('',#4829,#4830,#3038,.T.);
#5811=EDGE_CURVE('',#4830,#4831,#3039,.T.);
#5812=EDGE_CURVE('',#4831,#4832,#3040,.T.);
#5813=EDGE_CURVE('',#4829,#4832,#3041,.T.);
#5814=EDGE_CURVE('',#4830,#4833,#3042,.T.);
#5815=EDGE_CURVE('',#4833,#4834,#3043,.T.);
#5816=EDGE_CURVE('',#4834,#4831,#3044,.T.);
#5817=EDGE_CURVE('',#4833,#4835,#3045,.T.);
#5818=EDGE_CURVE('',#4835,#4836,#3046,.T.);
#5819=EDGE_CURVE('',#4836,#4834,#3047,.T.);
#5820=EDGE_CURVE('',#4835,#4837,#3048,.T.);
#5821=EDGE_CURVE('',#4837,#4838,#3049,.T.);
#5822=EDGE_CURVE('',#4838,#4836,#3050,.T.);
#5823=EDGE_CURVE('',#4837,#4839,#3051,.T.);
#5824=EDGE_CURVE('',#4839,#4840,#3052,.T.);
#5825=EDGE_CURVE('',#4840,#4838,#3053,.T.);
#5826=EDGE_CURVE('',#4839,#4829,#3054,.T.);
#5827=EDGE_CURVE('',#4832,#4840,#3055,.T.);
#5828=EDGE_CURVE('',#4841,#4841,#4134,.T.);
#5829=EDGE_CURVE('',#4842,#4842,#4135,.T.);
#5830=EDGE_CURVE('',#4843,#4843,#4136,.T.);
#5831=EDGE_CURVE('',#4843,#4842,#3056,.T.);
#5832=EDGE_CURVE('',#4844,#4844,#4137,.T.);
#5833=EDGE_CURVE('',#4844,#4843,#3057,.T.);
#5834=EDGE_CURVE('',#4845,#4845,#4138,.T.);
#5835=EDGE_CURVE('',#4845,#4844,#3058,.T.);
#5836=EDGE_CURVE('',#4846,#4846,#4139,.T.);
#5837=EDGE_CURVE('',#4847,#4847,#4140,.F.);
#5838=EDGE_CURVE('',#4847,#4846,#3059,.T.);
#5839=EDGE_CURVE('',#4841,#4847,#3060,.T.);
#5840=EDGE_CURVE('',#4848,#4848,#4141,.T.);
#5841=EDGE_CURVE('',#4849,#4849,#4142,.T.);
#5842=EDGE_CURVE('',#4849,#4848,#3061,.T.);
#5843=EDGE_CURVE('',#4850,#4850,#4143,.T.);
#5844=EDGE_CURVE('',#4850,#4849,#3062,.T.);
#5845=EDGE_CURVE('',#4851,#4851,#4144,.T.);
#5846=EDGE_CURVE('',#4851,#4850,#3063,.T.);
#5847=EDGE_CURVE('',#4852,#4852,#4145,.T.);
#5848=EDGE_CURVE('',#4853,#4853,#4146,.F.);
#5849=EDGE_CURVE('',#4853,#4852,#3064,.T.);
#5850=EDGE_CURVE('',#4854,#4854,#4147,.F.);
#5851=EDGE_CURVE('',#4854,#4853,#3065,.T.);
#5852=EDGE_CURVE('',#4855,#4855,#4148,.T.);
#5853=EDGE_CURVE('',#4855,#4854,#3066,.T.);
#5854=EDGE_CURVE('',#4856,#4857,#3067,.T.);
#5855=EDGE_CURVE('',#4857,#4858,#3068,.T.);
#5856=EDGE_CURVE('',#4858,#4859,#3069,.T.);
#5857=EDGE_CURVE('',#4856,#4859,#3070,.T.);
#5858=EDGE_CURVE('',#4857,#4860,#3071,.T.);
#5859=EDGE_CURVE('',#4860,#4861,#3072,.T.);
#5860=EDGE_CURVE('',#4861,#4858,#3073,.T.);
#5861=EDGE_CURVE('',#4860,#4862,#3074,.T.);
#5862=EDGE_CURVE('',#4862,#4863,#3075,.T.);
#5863=EDGE_CURVE('',#4863,#4861,#3076,.T.);
#5864=EDGE_CURVE('',#4862,#4864,#3077,.T.);
#5865=EDGE_CURVE('',#4864,#4865,#3078,.T.);
#5866=EDGE_CURVE('',#4865,#4863,#3079,.T.);
#5867=EDGE_CURVE('',#4864,#4866,#3080,.T.);
#5868=EDGE_CURVE('',#4866,#4867,#3081,.T.);
#5869=EDGE_CURVE('',#4867,#4865,#3082,.T.);
#5870=EDGE_CURVE('',#4866,#4856,#3083,.T.);
#5871=EDGE_CURVE('',#4859,#4867,#3084,.T.);
#5872=EDGE_CURVE('',#4868,#4868,#4149,.T.);
#5873=EDGE_CURVE('',#4868,#4869,#3085,.T.);
#5874=EDGE_CURVE('',#4869,#4869,#4150,.T.);
#5875=EDGE_CURVE('',#4870,#4870,#4151,.T.);
#5876=EDGE_CURVE('',#4870,#4871,#3086,.T.);
#5877=EDGE_CURVE('',#4871,#4871,#4152,.T.);
#5878=EDGE_CURVE('',#4872,#4872,#4153,.T.);
#5879=EDGE_CURVE('',#4872,#4873,#3087,.T.);
#5880=EDGE_CURVE('',#4873,#4873,#4154,.T.);
#5881=EDGE_CURVE('',#4874,#4874,#4155,.T.);
#5882=EDGE_CURVE('',#4874,#4875,#3088,.T.);
#5883=EDGE_CURVE('',#4875,#4875,#4156,.T.);
#5884=EDGE_CURVE('',#4876,#4876,#4157,.T.);
#5885=EDGE_CURVE('',#4876,#4877,#3089,.T.);
#5886=EDGE_CURVE('',#4877,#4877,#4158,.T.);
#5887=EDGE_CURVE('',#4878,#4878,#4159,.T.);
#5888=EDGE_CURVE('',#4878,#4879,#3090,.T.);
#5889=EDGE_CURVE('',#4879,#4879,#4160,.T.);
#5890=EDGE_CURVE('',#4880,#4880,#4161,.T.);
#5891=EDGE_CURVE('',#4880,#4881,#3091,.T.);
#5892=EDGE_CURVE('',#4881,#4881,#4162,.T.);
#5893=EDGE_CURVE('',#4882,#4882,#4163,.T.);
#5894=EDGE_CURVE('',#4882,#4883,#3092,.T.);
#5895=EDGE_CURVE('',#4883,#4883,#4164,.T.);
#5896=EDGE_CURVE('',#4884,#4884,#4165,.T.);
#5897=EDGE_CURVE('',#4884,#4885,#3093,.T.);
#5898=EDGE_CURVE('',#4885,#4885,#4166,.T.);
#5899=EDGE_CURVE('',#4886,#4886,#4167,.T.);
#5900=EDGE_CURVE('',#4886,#4887,#3094,.T.);
#5901=EDGE_CURVE('',#4887,#4887,#4168,.T.);
#5902=EDGE_CURVE('',#4888,#4888,#4169,.T.);
#5903=EDGE_CURVE('',#4888,#4889,#3095,.T.);
#5904=EDGE_CURVE('',#4889,#4889,#4170,.T.);
#5905=EDGE_CURVE('',#4890,#4890,#4171,.T.);
#5906=EDGE_CURVE('',#4890,#4891,#3096,.T.);
#5907=EDGE_CURVE('',#4891,#4891,#4172,.T.);
#5908=EDGE_CURVE('',#4892,#4892,#4173,.T.);
#5909=EDGE_CURVE('',#4892,#4893,#3097,.T.);
#5910=EDGE_CURVE('',#4893,#4893,#4174,.T.);
#5911=EDGE_CURVE('',#4894,#4894,#4175,.T.);
#5912=EDGE_CURVE('',#4894,#4895,#3098,.T.);
#5913=EDGE_CURVE('',#4895,#4895,#4176,.T.);
#5914=EDGE_CURVE('',#4896,#4896,#4177,.T.);
#5915=EDGE_CURVE('',#4896,#4897,#3099,.T.);
#5916=EDGE_CURVE('',#4897,#4897,#4178,.T.);
#5917=EDGE_CURVE('',#4898,#4898,#4179,.T.);
#5918=EDGE_CURVE('',#4898,#4899,#3100,.T.);
#5919=EDGE_CURVE('',#4899,#4899,#4180,.T.);
#5920=EDGE_CURVE('',#4900,#4900,#4181,.T.);
#5921=EDGE_CURVE('',#4900,#4901,#3101,.T.);
#5922=EDGE_CURVE('',#4901,#4901,#4182,.T.);
#5923=EDGE_CURVE('',#4902,#4902,#4183,.T.);
#5924=EDGE_CURVE('',#4902,#4903,#3102,.T.);
#5925=EDGE_CURVE('',#4903,#4903,#4184,.T.);
#5926=EDGE_CURVE('',#4904,#4904,#4185,.T.);
#5927=EDGE_CURVE('',#4904,#4905,#3103,.T.);
#5928=EDGE_CURVE('',#4905,#4905,#4186,.T.);
#5929=EDGE_CURVE('',#4906,#4906,#4187,.T.);
#5930=EDGE_CURVE('',#4906,#4907,#3104,.T.);
#5931=EDGE_CURVE('',#4907,#4907,#4188,.T.);
#5932=EDGE_CURVE('',#4908,#4908,#4189,.T.);
#5933=EDGE_CURVE('',#4908,#4909,#3105,.T.);
#5934=EDGE_CURVE('',#4909,#4909,#4190,.T.);
#5935=EDGE_CURVE('',#4910,#4910,#4191,.T.);
#5936=EDGE_CURVE('',#4910,#4911,#3106,.T.);
#5937=EDGE_CURVE('',#4911,#4911,#4192,.T.);
#5938=EDGE_CURVE('',#4912,#4912,#4193,.T.);
#5939=EDGE_CURVE('',#4912,#4913,#3107,.T.);
#5940=EDGE_CURVE('',#4913,#4913,#4194,.T.);
#5941=EDGE_CURVE('',#4914,#4914,#4195,.T.);
#5942=EDGE_CURVE('',#4914,#4915,#3108,.T.);
#5943=EDGE_CURVE('',#4915,#4915,#4196,.T.);
#5944=EDGE_CURVE('',#4916,#4917,#3109,.T.);
#5945=EDGE_CURVE('',#4917,#4918,#3110,.T.);
#5946=EDGE_CURVE('',#4919,#4918,#3111,.T.);
#5947=EDGE_CURVE('',#4916,#4919,#3112,.T.);
#5948=EDGE_CURVE('',#4920,#4916,#3113,.T.);
#5949=EDGE_CURVE('',#4921,#4919,#3114,.T.);
#5950=EDGE_CURVE('',#4920,#4921,#3115,.T.);
#5951=EDGE_CURVE('',#4922,#4920,#3116,.T.);
#5952=EDGE_CURVE('',#4923,#4921,#3117,.T.);
#5953=EDGE_CURVE('',#4922,#4923,#3118,.T.);
#5954=EDGE_CURVE('',#4917,#4922,#3119,.T.);
#5955=EDGE_CURVE('',#4918,#4923,#3120,.T.);
#5956=EDGE_CURVE('',#4924,#4925,#4197,.T.);
#5957=EDGE_CURVE('',#4924,#4925,#4198,.T.);
#5958=EDGE_CURVE('',#4926,#4924,#3121,.T.);
#5959=EDGE_CURVE('',#4927,#4926,#4199,.T.);
#5960=EDGE_CURVE('',#4927,#4928,#3122,.T.);
#5961=EDGE_CURVE('',#4928,#4928,#4200,.T.);
#5962=EDGE_CURVE('',#4929,#4927,#4201,.T.);
#5963=EDGE_CURVE('',#4925,#4929,#3123,.T.);
#5964=EDGE_CURVE('',#4930,#4931,#4202,.T.);
#5965=EDGE_CURVE('',#4930,#4931,#4203,.T.);
#5966=EDGE_CURVE('',#4932,#4930,#3124,.T.);
#5967=EDGE_CURVE('',#4933,#4932,#4204,.T.);
#5968=EDGE_CURVE('',#4933,#4934,#3125,.T.);
#5969=EDGE_CURVE('',#4934,#4934,#4205,.T.);
#5970=EDGE_CURVE('',#4935,#4933,#4206,.T.);
#5971=EDGE_CURVE('',#4931,#4935,#3126,.T.);
#5972=EDGE_CURVE('',#4936,#4937,#4207,.T.);
#5973=EDGE_CURVE('',#4936,#4938,#4208,.T.);
#5974=EDGE_CURVE('',#4938,#4937,#4209,.T.);
#5975=EDGE_CURVE('',#4939,#4936,#3127,.T.);
#5976=EDGE_CURVE('',#4940,#4939,#4210,.T.);
#5977=EDGE_CURVE('',#4937,#4940,#3128,.T.);
#5978=EDGE_CURVE('',#4938,#4941,#3129,.T.);
#5979=EDGE_CURVE('',#4941,#4941,#4211,.T.);
#5980=EDGE_CURVE('',#4942,#4943,#4212,.T.);
#5981=EDGE_CURVE('',#4942,#4944,#4213,.T.);
#5982=EDGE_CURVE('',#4944,#4943,#4214,.T.);
#5983=EDGE_CURVE('',#4945,#4942,#3130,.T.);
#5984=EDGE_CURVE('',#4946,#4945,#4215,.T.);
#5985=EDGE_CURVE('',#4943,#4946,#3131,.T.);
#5986=EDGE_CURVE('',#4944,#4947,#3132,.T.);
#5987=EDGE_CURVE('',#4947,#4947,#4216,.T.);
#5988=EDGE_CURVE('',#4929,#4948,#4217,.T.);
#5989=EDGE_CURVE('',#4948,#4949,#3133,.T.);
#5990=EDGE_CURVE('',#4949,#4949,#4218,.T.);
#5991=EDGE_CURVE('',#4948,#4932,#4219,.T.);
#5992=EDGE_CURVE('',#4935,#4939,#4220,.T.);
#5993=EDGE_CURVE('',#4940,#4945,#4221,.T.);
#5994=EDGE_CURVE('',#4946,#4926,#4222,.T.);
#5995=EDGE_CURVE('',#4950,#4950,#4223,.T.);
#5996=EDGE_CURVE('',#4950,#4951,#3134,.T.);
#5997=EDGE_CURVE('',#4951,#4951,#4224,.T.);
#5998=EDGE_CURVE('',#4952,#4952,#4225,.T.);
#5999=EDGE_CURVE('',#4953,#4953,#4226,.T.);
#6000=EDGE_CURVE('',#4954,#4954,#4227,.T.);
#6001=EDGE_CURVE('',#4954,#4953,#3135,.T.);
#6002=EDGE_CURVE('',#4952,#4955,#3136,.T.);
#6003=EDGE_CURVE('',#4955,#4955,#4228,.T.);
#6004=EDGE_CURVE('',#4956,#4957,#4229,.T.);
#6005=EDGE_CURVE('',#4956,#4957,#4230,.T.);
#6006=EDGE_CURVE('',#4958,#4956,#3137,.T.);
#6007=EDGE_CURVE('',#4959,#4958,#4231,.T.);
#6008=EDGE_CURVE('',#4959,#4960,#3138,.T.);
#6009=EDGE_CURVE('',#4960,#4960,#4232,.T.);
#6010=EDGE_CURVE('',#4961,#4959,#4233,.T.);
#6011=EDGE_CURVE('',#4957,#4961,#3139,.T.);
#6012=EDGE_CURVE('',#4962,#4963,#4234,.T.);
#6013=EDGE_CURVE('',#4962,#4963,#4235,.T.);
#6014=EDGE_CURVE('',#4964,#4962,#3140,.T.);
#6015=EDGE_CURVE('',#4965,#4964,#4236,.T.);
#6016=EDGE_CURVE('',#4965,#4966,#3141,.T.);
#6017=EDGE_CURVE('',#4966,#4966,#4237,.T.);
#6018=EDGE_CURVE('',#4967,#4965,#4238,.T.);
#6019=EDGE_CURVE('',#4963,#4967,#3142,.T.);
#6020=EDGE_CURVE('',#4968,#4969,#4239,.T.);
#6021=EDGE_CURVE('',#4968,#4970,#4240,.T.);
#6022=EDGE_CURVE('',#4970,#4969,#4241,.T.);
#6023=EDGE_CURVE('',#4971,#4968,#3143,.T.);
#6024=EDGE_CURVE('',#4972,#4971,#4242,.T.);
#6025=EDGE_CURVE('',#4969,#4972,#3144,.T.);
#6026=EDGE_CURVE('',#4970,#4973,#3145,.T.);
#6027=EDGE_CURVE('',#4973,#4973,#4243,.T.);
#6028=EDGE_CURVE('',#4974,#4975,#4244,.T.);
#6029=EDGE_CURVE('',#4974,#4976,#4245,.T.);
#6030=EDGE_CURVE('',#4976,#4975,#4246,.T.);
#6031=EDGE_CURVE('',#4977,#4974,#3146,.T.);
#6032=EDGE_CURVE('',#4978,#4977,#4247,.T.);
#6033=EDGE_CURVE('',#4975,#4978,#3147,.T.);
#6034=EDGE_CURVE('',#4976,#4979,#3148,.T.);
#6035=EDGE_CURVE('',#4979,#4979,#4248,.T.);
#6036=EDGE_CURVE('',#4961,#4980,#4249,.T.);
#6037=EDGE_CURVE('',#4980,#4981,#3149,.T.);
#6038=EDGE_CURVE('',#4981,#4981,#4250,.T.);
#6039=EDGE_CURVE('',#4980,#4964,#4251,.T.);
#6040=EDGE_CURVE('',#4967,#4971,#4252,.T.);
#6041=EDGE_CURVE('',#4972,#4977,#4253,.T.);
#6042=EDGE_CURVE('',#4978,#4958,#4254,.T.);
#6043=EDGE_CURVE('',#4982,#4982,#4255,.T.);
#6044=EDGE_CURVE('',#4982,#4983,#3150,.T.);
#6045=EDGE_CURVE('',#4983,#4983,#4256,.T.);
#6046=EDGE_CURVE('',#4984,#4984,#4257,.T.);
#6047=EDGE_CURVE('',#4985,#4985,#4258,.T.);
#6048=EDGE_CURVE('',#4986,#4986,#4259,.T.);
#6049=EDGE_CURVE('',#4986,#4985,#3151,.T.);
#6050=EDGE_CURVE('',#4984,#4987,#3152,.T.);
#6051=EDGE_CURVE('',#4987,#4987,#4260,.T.);
#6052=EDGE_CURVE('',#4988,#4989,#4261,.T.);
#6053=EDGE_CURVE('',#4988,#4989,#4262,.T.);
#6054=EDGE_CURVE('',#4990,#4988,#3153,.T.);
#6055=EDGE_CURVE('',#4991,#4990,#4263,.T.);
#6056=EDGE_CURVE('',#4991,#4992,#3154,.T.);
#6057=EDGE_CURVE('',#4992,#4992,#4264,.T.);
#6058=EDGE_CURVE('',#4993,#4991,#4265,.T.);
#6059=EDGE_CURVE('',#4989,#4993,#3155,.T.);
#6060=EDGE_CURVE('',#4994,#4995,#4266,.T.);
#6061=EDGE_CURVE('',#4994,#4995,#4267,.T.);
#6062=EDGE_CURVE('',#4996,#4994,#3156,.T.);
#6063=EDGE_CURVE('',#4997,#4996,#4268,.T.);
#6064=EDGE_CURVE('',#4997,#4998,#3157,.T.);
#6065=EDGE_CURVE('',#4998,#4998,#4269,.T.);
#6066=EDGE_CURVE('',#4999,#4997,#4270,.T.);
#6067=EDGE_CURVE('',#4995,#4999,#3158,.T.);
#6068=EDGE_CURVE('',#5000,#5001,#4271,.T.);
#6069=EDGE_CURVE('',#5000,#5002,#4272,.T.);
#6070=EDGE_CURVE('',#5002,#5001,#4273,.T.);
#6071=EDGE_CURVE('',#5003,#5000,#3159,.T.);
#6072=EDGE_CURVE('',#5004,#5003,#4274,.T.);
#6073=EDGE_CURVE('',#5001,#5004,#3160,.T.);
#6074=EDGE_CURVE('',#5002,#5005,#3161,.T.);
#6075=EDGE_CURVE('',#5005,#5005,#4275,.T.);
#6076=EDGE_CURVE('',#5006,#5007,#4276,.T.);
#6077=EDGE_CURVE('',#5006,#5008,#4277,.T.);
#6078=EDGE_CURVE('',#5008,#5007,#4278,.T.);
#6079=EDGE_CURVE('',#5009,#5006,#3162,.T.);
#6080=EDGE_CURVE('',#5010,#5009,#4279,.T.);
#6081=EDGE_CURVE('',#5007,#5010,#3163,.T.);
#6082=EDGE_CURVE('',#5008,#5011,#3164,.T.);
#6083=EDGE_CURVE('',#5011,#5011,#4280,.T.);
#6084=EDGE_CURVE('',#4993,#5012,#4281,.T.);
#6085=EDGE_CURVE('',#5012,#5013,#3165,.T.);
#6086=EDGE_CURVE('',#5013,#5013,#4282,.T.);
#6087=EDGE_CURVE('',#5012,#4996,#4283,.T.);
#6088=EDGE_CURVE('',#4999,#5003,#4284,.T.);
#6089=EDGE_CURVE('',#5004,#5009,#4285,.T.);
#6090=EDGE_CURVE('',#5010,#4990,#4286,.T.);
#6091=EDGE_CURVE('',#5014,#5014,#4287,.T.);
#6092=EDGE_CURVE('',#5014,#5015,#3166,.T.);
#6093=EDGE_CURVE('',#5015,#5015,#4288,.T.);
#6094=EDGE_CURVE('',#5016,#5016,#4289,.T.);
#6095=EDGE_CURVE('',#5017,#5017,#4290,.T.);
#6096=EDGE_CURVE('',#5018,#5018,#4291,.T.);
#6097=EDGE_CURVE('',#5018,#5017,#3167,.T.);
#6098=EDGE_CURVE('',#5016,#5019,#3168,.T.);
#6099=EDGE_CURVE('',#5019,#5019,#4292,.T.);
#6100=EDGE_CURVE('',#5020,#5021,#4293,.T.);
#6101=EDGE_CURVE('',#5020,#5021,#4294,.T.);
#6102=EDGE_CURVE('',#5022,#5020,#3169,.T.);
#6103=EDGE_CURVE('',#5023,#5022,#4295,.T.);
#6104=EDGE_CURVE('',#5023,#5024,#3170,.T.);
#6105=EDGE_CURVE('',#5024,#5024,#4296,.T.);
#6106=EDGE_CURVE('',#5025,#5023,#4297,.T.);
#6107=EDGE_CURVE('',#5021,#5025,#3171,.T.);
#6108=EDGE_CURVE('',#5026,#5027,#4298,.T.);
#6109=EDGE_CURVE('',#5026,#5027,#4299,.T.);
#6110=EDGE_CURVE('',#5028,#5026,#3172,.T.);
#6111=EDGE_CURVE('',#5029,#5028,#4300,.T.);
#6112=EDGE_CURVE('',#5029,#5030,#3173,.T.);
#6113=EDGE_CURVE('',#5030,#5030,#4301,.T.);
#6114=EDGE_CURVE('',#5031,#5029,#4302,.T.);
#6115=EDGE_CURVE('',#5027,#5031,#3174,.T.);
#6116=EDGE_CURVE('',#5032,#5033,#4303,.T.);
#6117=EDGE_CURVE('',#5032,#5034,#4304,.T.);
#6118=EDGE_CURVE('',#5034,#5033,#4305,.T.);
#6119=EDGE_CURVE('',#5035,#5032,#3175,.T.);
#6120=EDGE_CURVE('',#5036,#5035,#4306,.T.);
#6121=EDGE_CURVE('',#5033,#5036,#3176,.T.);
#6122=EDGE_CURVE('',#5034,#5037,#3177,.T.);
#6123=EDGE_CURVE('',#5037,#5037,#4307,.T.);
#6124=EDGE_CURVE('',#5038,#5039,#4308,.T.);
#6125=EDGE_CURVE('',#5038,#5040,#4309,.T.);
#6126=EDGE_CURVE('',#5040,#5039,#4310,.T.);
#6127=EDGE_CURVE('',#5041,#5038,#3178,.T.);
#6128=EDGE_CURVE('',#5042,#5041,#4311,.T.);
#6129=EDGE_CURVE('',#5039,#5042,#3179,.T.);
#6130=EDGE_CURVE('',#5040,#5043,#3180,.T.);
#6131=EDGE_CURVE('',#5043,#5043,#4312,.T.);
#6132=EDGE_CURVE('',#5025,#5044,#4313,.T.);
#6133=EDGE_CURVE('',#5044,#5045,#3181,.T.);
#6134=EDGE_CURVE('',#5045,#5045,#4314,.T.);
#6135=EDGE_CURVE('',#5044,#5028,#4315,.T.);
#6136=EDGE_CURVE('',#5031,#5035,#4316,.T.);
#6137=EDGE_CURVE('',#5036,#5041,#4317,.T.);
#6138=EDGE_CURVE('',#5042,#5022,#4318,.T.);
#6139=EDGE_CURVE('',#5046,#5046,#4319,.T.);
#6140=EDGE_CURVE('',#5046,#5047,#3182,.T.);
#6141=EDGE_CURVE('',#5047,#5047,#4320,.T.);
#6142=EDGE_CURVE('',#5048,#5048,#4321,.T.);
#6143=EDGE_CURVE('',#5049,#5049,#4322,.T.);
#6144=EDGE_CURVE('',#5050,#5050,#4323,.T.);
#6145=EDGE_CURVE('',#5050,#5049,#3183,.T.);
#6146=EDGE_CURVE('',#5048,#5051,#3184,.T.);
#6147=EDGE_CURVE('',#5051,#5051,#4324,.T.);
#6148=EDGE_CURVE('',#5052,#5052,#4325,.T.);
#6149=EDGE_CURVE('',#5052,#5053,#3185,.T.);
#6150=EDGE_CURVE('',#5053,#5053,#4326,.T.);
#6151=EDGE_CURVE('',#5054,#5054,#4327,.T.);
#6152=EDGE_CURVE('',#5054,#5055,#3186,.T.);
#6153=EDGE_CURVE('',#5055,#5055,#4328,.T.);
#6154=EDGE_CURVE('',#5056,#5056,#4329,.T.);
#6155=EDGE_CURVE('',#5056,#5057,#3187,.T.);
#6156=EDGE_CURVE('',#5057,#5057,#4330,.T.);
#6157=EDGE_CURVE('',#5058,#5058,#4331,.T.);
#6158=EDGE_CURVE('',#5058,#5059,#3188,.T.);
#6159=EDGE_CURVE('',#5059,#5059,#4332,.T.);
#6160=EDGE_CURVE('',#5060,#5060,#4333,.T.);
#6161=EDGE_CURVE('',#5061,#5061,#4334,.T.);
#6162=EDGE_CURVE('',#5062,#5062,#4335,.T.);
#6163=EDGE_CURVE('',#5062,#5060,#3189,.T.);
#6164=EDGE_CURVE('',#5061,#5063,#3190,.T.);
#6165=EDGE_CURVE('',#5063,#5063,#4336,.T.);
#6166=EDGE_CURVE('',#5064,#5065,#4337,.T.);
#6167=EDGE_CURVE('',#5066,#5064,#3191,.T.);
#6168=EDGE_CURVE('',#5067,#5066,#3192,.T.);
#6169=EDGE_CURVE('',#5065,#5067,#3193,.T.);
#6170=EDGE_CURVE('',#5065,#5068,#3194,.T.);
#6171=EDGE_CURVE('',#5069,#5067,#3195,.T.);
#6172=EDGE_CURVE('',#5069,#5068,#3196,.T.);
#6173=EDGE_CURVE('',#5068,#5070,#4338,.T.);
#6174=EDGE_CURVE('',#5071,#5069,#3197,.T.);
#6175=EDGE_CURVE('',#5070,#5071,#3198,.T.);
#6176=EDGE_CURVE('',#5070,#5064,#3199,.T.);
#6177=EDGE_CURVE('',#5071,#5066,#3200,.T.);
#6178=EDGE_CURVE('',#5072,#5072,#4339,.T.);
#6179=EDGE_CURVE('',#5073,#5073,#4340,.T.);
#6180=EDGE_CURVE('',#5074,#5074,#4341,.T.);
#6181=EDGE_CURVE('',#5074,#5072,#3201,.T.);
#6182=EDGE_CURVE('',#5075,#5075,#4342,.T.);
#6183=EDGE_CURVE('',#5076,#5076,#4343,.T.);
#6184=EDGE_CURVE('',#5076,#5075,#3202,.T.);
#6185=EDGE_CURVE('',#5077,#5077,#4344,.T.);
#6186=EDGE_CURVE('',#5078,#5078,#4345,.T.);
#6187=EDGE_CURVE('',#5078,#5077,#3203,.T.);
#6188=EDGE_CURVE('',#5079,#5079,#4346,.T.);
#6189=EDGE_CURVE('',#5080,#5080,#4347,.T.);
#6190=EDGE_CURVE('',#5080,#5079,#3204,.T.);
#6191=EDGE_CURVE('',#5081,#5081,#4348,.T.);
#6192=EDGE_CURVE('',#5082,#5082,#4349,.T.);
#6193=EDGE_CURVE('',#5082,#5081,#3205,.T.);
#6194=EDGE_CURVE('',#5083,#5083,#4350,.T.);
#6195=EDGE_CURVE('',#5083,#5073,#3206,.T.);
#6196=EDGE_CURVE('',#5084,#5085,#4351,.T.);
#6197=EDGE_CURVE('',#5086,#5084,#3207,.T.);
#6198=EDGE_CURVE('',#5087,#5086,#4352,.T.);
#6199=EDGE_CURVE('',#5085,#5087,#3208,.T.);
#6200=EDGE_CURVE('',#5085,#5088,#3209,.T.);
#6201=EDGE_CURVE('',#5089,#5087,#3210,.T.);
#6202=EDGE_CURVE('',#5089,#5088,#3211,.T.);
#6203=EDGE_CURVE('',#5088,#5090,#4353,.T.);
#6204=EDGE_CURVE('',#5091,#5089,#4354,.T.);
#6205=EDGE_CURVE('',#5090,#5091,#3212,.T.);
#6206=EDGE_CURVE('',#5090,#5084,#3213,.T.);
#6207=EDGE_CURVE('',#5086,#5091,#3214,.T.);
#6208=EDGE_CURVE('',#5092,#5092,#4355,.T.);
#6209=EDGE_CURVE('',#5093,#5093,#4356,.T.);
#6210=EDGE_CURVE('',#5094,#5094,#4357,.T.);
#6211=EDGE_CURVE('',#5094,#5092,#3215,.T.);
#6212=EDGE_CURVE('',#5095,#5095,#4358,.T.);
#6213=EDGE_CURVE('',#5095,#5093,#3216,.T.);
#6214=EDGE_CURVE('',#5096,#5096,#4359,.T.);
#6215=EDGE_CURVE('',#5097,#5097,#4360,.T.);
#6216=EDGE_CURVE('',#5097,#5096,#3217,.T.);
#6217=EDGE_CURVE('',#5098,#5098,#4361,.T.);
#6218=EDGE_CURVE('',#5098,#5097,#3218,.T.);
#6219=EDGE_CURVE('',#5099,#5099,#4362,.T.);
#6220=EDGE_CURVE('',#5099,#5098,#3219,.T.);
#6221=EDGE_CURVE('',#5100,#5100,#4363,.T.);
#6222=EDGE_CURVE('',#5101,#5101,#4364,.F.);
#6223=EDGE_CURVE('',#5101,#5100,#3220,.T.);
#6224=EDGE_CURVE('',#5102,#5102,#4365,.F.);
#6225=EDGE_CURVE('',#5102,#5101,#3221,.T.);
#6226=EDGE_CURVE('',#5103,#5103,#4366,.T.);
#6227=EDGE_CURVE('',#5103,#5102,#3222,.T.);
#6228=EDGE_CURVE('',#5104,#5105,#3223,.T.);
#6229=EDGE_CURVE('',#5105,#5106,#3224,.T.);
#6230=EDGE_CURVE('',#5106,#5107,#3225,.T.);
#6231=EDGE_CURVE('',#5104,#5107,#3226,.T.);
#6232=EDGE_CURVE('',#5105,#5108,#3227,.T.);
#6233=EDGE_CURVE('',#5108,#5109,#3228,.T.);
#6234=EDGE_CURVE('',#5109,#5106,#3229,.T.);
#6235=EDGE_CURVE('',#5108,#5110,#3230,.T.);
#6236=EDGE_CURVE('',#5110,#5111,#3231,.T.);
#6237=EDGE_CURVE('',#5111,#5109,#3232,.T.);
#6238=EDGE_CURVE('',#5110,#5112,#3233,.T.);
#6239=EDGE_CURVE('',#5112,#5113,#3234,.T.);
#6240=EDGE_CURVE('',#5113,#5111,#3235,.T.);
#6241=EDGE_CURVE('',#5112,#5114,#3236,.T.);
#6242=EDGE_CURVE('',#5114,#5115,#3237,.T.);
#6243=EDGE_CURVE('',#5115,#5113,#3238,.T.);
#6244=EDGE_CURVE('',#5114,#5104,#3239,.T.);
#6245=EDGE_CURVE('',#5107,#5115,#3240,.T.);
#6246=ORIENTED_EDGE('',*,*,#5116,.F.);
#6247=ORIENTED_EDGE('',*,*,#5117,.T.);
#6248=ORIENTED_EDGE('',*,*,#5118,.F.);
#6249=ORIENTED_EDGE('',*,*,#5117,.F.);
#6250=ORIENTED_EDGE('',*,*,#5119,.F.);
#6251=ORIENTED_EDGE('',*,*,#5120,.T.);
#6252=ORIENTED_EDGE('',*,*,#5121,.F.);
#6253=ORIENTED_EDGE('',*,*,#5120,.F.);
#6254=ORIENTED_EDGE('',*,*,#5122,.F.);
#6255=ORIENTED_EDGE('',*,*,#5123,.T.);
#6256=ORIENTED_EDGE('',*,*,#5124,.F.);
#6257=ORIENTED_EDGE('',*,*,#5123,.F.);
#6258=ORIENTED_EDGE('',*,*,#5125,.F.);
#6259=ORIENTED_EDGE('',*,*,#5126,.T.);
#6260=ORIENTED_EDGE('',*,*,#5127,.F.);
#6261=ORIENTED_EDGE('',*,*,#5126,.F.);
#6262=ORIENTED_EDGE('',*,*,#5128,.F.);
#6263=ORIENTED_EDGE('',*,*,#5129,.T.);
#6264=ORIENTED_EDGE('',*,*,#5130,.F.);
#6265=ORIENTED_EDGE('',*,*,#5129,.F.);
#6266=ORIENTED_EDGE('',*,*,#5131,.F.);
#6267=ORIENTED_EDGE('',*,*,#5132,.T.);
#6268=ORIENTED_EDGE('',*,*,#5133,.F.);
#6269=ORIENTED_EDGE('',*,*,#5132,.F.);
#6270=ORIENTED_EDGE('',*,*,#5134,.F.);
#6271=ORIENTED_EDGE('',*,*,#5135,.T.);
#6272=ORIENTED_EDGE('',*,*,#5136,.F.);
#6273=ORIENTED_EDGE('',*,*,#5135,.F.);
#6274=ORIENTED_EDGE('',*,*,#5137,.F.);
#6275=ORIENTED_EDGE('',*,*,#5138,.T.);
#6276=ORIENTED_EDGE('',*,*,#5139,.F.);
#6277=ORIENTED_EDGE('',*,*,#5138,.F.);
#6278=ORIENTED_EDGE('',*,*,#5140,.F.);
#6279=ORIENTED_EDGE('',*,*,#5141,.T.);
#6280=ORIENTED_EDGE('',*,*,#5142,.F.);
#6281=ORIENTED_EDGE('',*,*,#5141,.F.);
#6282=ORIENTED_EDGE('',*,*,#5143,.F.);
#6283=ORIENTED_EDGE('',*,*,#5144,.T.);
#6284=ORIENTED_EDGE('',*,*,#5145,.F.);
#6285=ORIENTED_EDGE('',*,*,#5144,.F.);
#6286=ORIENTED_EDGE('',*,*,#5146,.F.);
#6287=ORIENTED_EDGE('',*,*,#5147,.T.);
#6288=ORIENTED_EDGE('',*,*,#5148,.F.);
#6289=ORIENTED_EDGE('',*,*,#5147,.F.);
#6290=ORIENTED_EDGE('',*,*,#5149,.F.);
#6291=ORIENTED_EDGE('',*,*,#5150,.T.);
#6292=ORIENTED_EDGE('',*,*,#5151,.F.);
#6293=ORIENTED_EDGE('',*,*,#5150,.F.);
#6294=ORIENTED_EDGE('',*,*,#5152,.F.);
#6295=ORIENTED_EDGE('',*,*,#5153,.T.);
#6296=ORIENTED_EDGE('',*,*,#5154,.F.);
#6297=ORIENTED_EDGE('',*,*,#5153,.F.);
#6298=ORIENTED_EDGE('',*,*,#5155,.F.);
#6299=ORIENTED_EDGE('',*,*,#5156,.T.);
#6300=ORIENTED_EDGE('',*,*,#5157,.F.);
#6301=ORIENTED_EDGE('',*,*,#5156,.F.);
#6302=ORIENTED_EDGE('',*,*,#5158,.F.);
#6303=ORIENTED_EDGE('',*,*,#5159,.T.);
#6304=ORIENTED_EDGE('',*,*,#5160,.F.);
#6305=ORIENTED_EDGE('',*,*,#5159,.F.);
#6306=ORIENTED_EDGE('',*,*,#5161,.F.);
#6307=ORIENTED_EDGE('',*,*,#5162,.T.);
#6308=ORIENTED_EDGE('',*,*,#5163,.F.);
#6309=ORIENTED_EDGE('',*,*,#5162,.F.);
#6310=ORIENTED_EDGE('',*,*,#5164,.F.);
#6311=ORIENTED_EDGE('',*,*,#5165,.T.);
#6312=ORIENTED_EDGE('',*,*,#5166,.F.);
#6313=ORIENTED_EDGE('',*,*,#5165,.F.);
#6314=ORIENTED_EDGE('',*,*,#5167,.F.);
#6315=ORIENTED_EDGE('',*,*,#5168,.T.);
#6316=ORIENTED_EDGE('',*,*,#5169,.F.);
#6317=ORIENTED_EDGE('',*,*,#5168,.F.);
#6318=ORIENTED_EDGE('',*,*,#5170,.F.);
#6319=ORIENTED_EDGE('',*,*,#5171,.T.);
#6320=ORIENTED_EDGE('',*,*,#5172,.F.);
#6321=ORIENTED_EDGE('',*,*,#5171,.F.);
#6322=ORIENTED_EDGE('',*,*,#5173,.F.);
#6323=ORIENTED_EDGE('',*,*,#5174,.T.);
#6324=ORIENTED_EDGE('',*,*,#5175,.F.);
#6325=ORIENTED_EDGE('',*,*,#5174,.F.);
#6326=ORIENTED_EDGE('',*,*,#5176,.F.);
#6327=ORIENTED_EDGE('',*,*,#5177,.T.);
#6328=ORIENTED_EDGE('',*,*,#5178,.F.);
#6329=ORIENTED_EDGE('',*,*,#5177,.F.);
#6330=ORIENTED_EDGE('',*,*,#5179,.F.);
#6331=ORIENTED_EDGE('',*,*,#5180,.T.);
#6332=ORIENTED_EDGE('',*,*,#5181,.F.);
#6333=ORIENTED_EDGE('',*,*,#5180,.F.);
#6334=ORIENTED_EDGE('',*,*,#5182,.T.);
#6335=ORIENTED_EDGE('',*,*,#5183,.T.);
#6336=ORIENTED_EDGE('',*,*,#5184,.F.);
#6337=ORIENTED_EDGE('',*,*,#5185,.F.);
#6338=ORIENTED_EDGE('',*,*,#5186,.T.);
#6339=ORIENTED_EDGE('',*,*,#5185,.T.);
#6340=ORIENTED_EDGE('',*,*,#5187,.F.);
#6341=ORIENTED_EDGE('',*,*,#5188,.F.);
#6342=ORIENTED_EDGE('',*,*,#5189,.T.);
#6343=ORIENTED_EDGE('',*,*,#5188,.T.);
#6344=ORIENTED_EDGE('',*,*,#5190,.F.);
#6345=ORIENTED_EDGE('',*,*,#5191,.F.);
#6346=ORIENTED_EDGE('',*,*,#5192,.T.);
#6347=ORIENTED_EDGE('',*,*,#5191,.T.);
#6348=ORIENTED_EDGE('',*,*,#5193,.F.);
#6349=ORIENTED_EDGE('',*,*,#5183,.F.);
#6350=ORIENTED_EDGE('',*,*,#5193,.T.);
#6351=ORIENTED_EDGE('',*,*,#5190,.T.);
#6352=ORIENTED_EDGE('',*,*,#5187,.T.);
#6353=ORIENTED_EDGE('',*,*,#5184,.T.);
#6354=ORIENTED_EDGE('',*,*,#5121,.T.);
#6355=ORIENTED_EDGE('',*,*,#5136,.T.);
#6356=ORIENTED_EDGE('',*,*,#5139,.T.);
#6357=ORIENTED_EDGE('',*,*,#5142,.T.);
#6358=ORIENTED_EDGE('',*,*,#5145,.T.);
#6359=ORIENTED_EDGE('',*,*,#5154,.T.);
#6360=ORIENTED_EDGE('',*,*,#5157,.T.);
#6361=ORIENTED_EDGE('',*,*,#5181,.T.);
#6362=ORIENTED_EDGE('',*,*,#5178,.T.);
#6363=ORIENTED_EDGE('',*,*,#5175,.T.);
#6364=ORIENTED_EDGE('',*,*,#5172,.T.);
#6365=ORIENTED_EDGE('',*,*,#5169,.T.);
#6366=ORIENTED_EDGE('',*,*,#5166,.T.);
#6367=ORIENTED_EDGE('',*,*,#5163,.T.);
#6368=ORIENTED_EDGE('',*,*,#5160,.T.);
#6369=ORIENTED_EDGE('',*,*,#5151,.T.);
#6370=ORIENTED_EDGE('',*,*,#5148,.T.);
#6371=ORIENTED_EDGE('',*,*,#5133,.T.);
#6372=ORIENTED_EDGE('',*,*,#5130,.T.);
#6373=ORIENTED_EDGE('',*,*,#5127,.T.);
#6374=ORIENTED_EDGE('',*,*,#5124,.T.);
#6375=ORIENTED_EDGE('',*,*,#5118,.T.);
#6376=ORIENTED_EDGE('',*,*,#5192,.F.);
#6377=ORIENTED_EDGE('',*,*,#5182,.F.);
#6378=ORIENTED_EDGE('',*,*,#5186,.F.);
#6379=ORIENTED_EDGE('',*,*,#5189,.F.);
#6380=ORIENTED_EDGE('',*,*,#5119,.T.);
#6381=ORIENTED_EDGE('',*,*,#5134,.T.);
#6382=ORIENTED_EDGE('',*,*,#5137,.T.);
#6383=ORIENTED_EDGE('',*,*,#5140,.T.);
#6384=ORIENTED_EDGE('',*,*,#5143,.T.);
#6385=ORIENTED_EDGE('',*,*,#5152,.T.);
#6386=ORIENTED_EDGE('',*,*,#5155,.T.);
#6387=ORIENTED_EDGE('',*,*,#5179,.T.);
#6388=ORIENTED_EDGE('',*,*,#5176,.T.);
#6389=ORIENTED_EDGE('',*,*,#5173,.T.);
#6390=ORIENTED_EDGE('',*,*,#5170,.T.);
#6391=ORIENTED_EDGE('',*,*,#5167,.T.);
#6392=ORIENTED_EDGE('',*,*,#5164,.T.);
#6393=ORIENTED_EDGE('',*,*,#5161,.T.);
#6394=ORIENTED_EDGE('',*,*,#5158,.T.);
#6395=ORIENTED_EDGE('',*,*,#5149,.T.);
#6396=ORIENTED_EDGE('',*,*,#5146,.T.);
#6397=ORIENTED_EDGE('',*,*,#5131,.T.);
#6398=ORIENTED_EDGE('',*,*,#5128,.T.);
#6399=ORIENTED_EDGE('',*,*,#5125,.T.);
#6400=ORIENTED_EDGE('',*,*,#5122,.T.);
#6401=ORIENTED_EDGE('',*,*,#5116,.T.);
#6402=ORIENTED_EDGE('',*,*,#5194,.T.);
#6403=ORIENTED_EDGE('',*,*,#5195,.T.);
#6404=ORIENTED_EDGE('',*,*,#5196,.F.);
#6405=ORIENTED_EDGE('',*,*,#5197,.F.);
#6406=ORIENTED_EDGE('',*,*,#5198,.T.);
#6407=ORIENTED_EDGE('',*,*,#5197,.T.);
#6408=ORIENTED_EDGE('',*,*,#5199,.F.);
#6409=ORIENTED_EDGE('',*,*,#5200,.F.);
#6410=ORIENTED_EDGE('',*,*,#5201,.T.);
#6411=ORIENTED_EDGE('',*,*,#5200,.T.);
#6412=ORIENTED_EDGE('',*,*,#5202,.F.);
#6413=ORIENTED_EDGE('',*,*,#5203,.F.);
#6414=ORIENTED_EDGE('',*,*,#5204,.T.);
#6415=ORIENTED_EDGE('',*,*,#5203,.T.);
#6416=ORIENTED_EDGE('',*,*,#5205,.F.);
#6417=ORIENTED_EDGE('',*,*,#5195,.F.);
#6418=ORIENTED_EDGE('',*,*,#5205,.T.);
#6419=ORIENTED_EDGE('',*,*,#5202,.T.);
#6420=ORIENTED_EDGE('',*,*,#5199,.T.);
#6421=ORIENTED_EDGE('',*,*,#5196,.T.);
#6422=ORIENTED_EDGE('',*,*,#5204,.F.);
#6423=ORIENTED_EDGE('',*,*,#5194,.F.);
#6424=ORIENTED_EDGE('',*,*,#5198,.F.);
#6425=ORIENTED_EDGE('',*,*,#5201,.F.);
#6426=ORIENTED_EDGE('',*,*,#5206,.T.);
#6427=ORIENTED_EDGE('',*,*,#5207,.T.);
#6428=ORIENTED_EDGE('',*,*,#5208,.F.);
#6429=ORIENTED_EDGE('',*,*,#5209,.F.);
#6430=ORIENTED_EDGE('',*,*,#5210,.T.);
#6431=ORIENTED_EDGE('',*,*,#5209,.T.);
#6432=ORIENTED_EDGE('',*,*,#5211,.F.);
#6433=ORIENTED_EDGE('',*,*,#5212,.F.);
#6434=ORIENTED_EDGE('',*,*,#5213,.T.);
#6435=ORIENTED_EDGE('',*,*,#5212,.T.);
#6436=ORIENTED_EDGE('',*,*,#5214,.F.);
#6437=ORIENTED_EDGE('',*,*,#5215,.F.);
#6438=ORIENTED_EDGE('',*,*,#5216,.T.);
#6439=ORIENTED_EDGE('',*,*,#5215,.T.);
#6440=ORIENTED_EDGE('',*,*,#5217,.F.);
#6441=ORIENTED_EDGE('',*,*,#5207,.F.);
#6442=ORIENTED_EDGE('',*,*,#5217,.T.);
#6443=ORIENTED_EDGE('',*,*,#5214,.T.);
#6444=ORIENTED_EDGE('',*,*,#5211,.T.);
#6445=ORIENTED_EDGE('',*,*,#5208,.T.);
#6446=ORIENTED_EDGE('',*,*,#5216,.F.);
#6447=ORIENTED_EDGE('',*,*,#5206,.F.);
#6448=ORIENTED_EDGE('',*,*,#5210,.F.);
#6449=ORIENTED_EDGE('',*,*,#5213,.F.);
#6450=ORIENTED_EDGE('',*,*,#5218,.F.);
#6451=ORIENTED_EDGE('',*,*,#5219,.T.);
#6452=ORIENTED_EDGE('',*,*,#5220,.F.);
#6453=ORIENTED_EDGE('',*,*,#5219,.F.);
#6454=ORIENTED_EDGE('',*,*,#5221,.F.);
#6455=ORIENTED_EDGE('',*,*,#5222,.T.);
#6456=ORIENTED_EDGE('',*,*,#5223,.F.);
#6457=ORIENTED_EDGE('',*,*,#5222,.F.);
#6458=ORIENTED_EDGE('',*,*,#5224,.F.);
#6459=ORIENTED_EDGE('',*,*,#5225,.T.);
#6460=ORIENTED_EDGE('',*,*,#5226,.F.);
#6461=ORIENTED_EDGE('',*,*,#5225,.F.);
#6462=ORIENTED_EDGE('',*,*,#5227,.F.);
#6463=ORIENTED_EDGE('',*,*,#5228,.T.);
#6464=ORIENTED_EDGE('',*,*,#5229,.F.);
#6465=ORIENTED_EDGE('',*,*,#5228,.F.);
#6466=ORIENTED_EDGE('',*,*,#5230,.F.);
#6467=ORIENTED_EDGE('',*,*,#5231,.T.);
#6468=ORIENTED_EDGE('',*,*,#5232,.F.);
#6469=ORIENTED_EDGE('',*,*,#5231,.F.);
#6470=ORIENTED_EDGE('',*,*,#5233,.F.);
#6471=ORIENTED_EDGE('',*,*,#5234,.T.);
#6472=ORIENTED_EDGE('',*,*,#5235,.F.);
#6473=ORIENTED_EDGE('',*,*,#5234,.F.);
#6474=ORIENTED_EDGE('',*,*,#5236,.F.);
#6475=ORIENTED_EDGE('',*,*,#5237,.T.);
#6476=ORIENTED_EDGE('',*,*,#5238,.F.);
#6477=ORIENTED_EDGE('',*,*,#5237,.F.);
#6478=ORIENTED_EDGE('',*,*,#5239,.F.);
#6479=ORIENTED_EDGE('',*,*,#5240,.T.);
#6480=ORIENTED_EDGE('',*,*,#5241,.F.);
#6481=ORIENTED_EDGE('',*,*,#5240,.F.);
#6482=ORIENTED_EDGE('',*,*,#5242,.F.);
#6483=ORIENTED_EDGE('',*,*,#5243,.T.);
#6484=ORIENTED_EDGE('',*,*,#5244,.F.);
#6485=ORIENTED_EDGE('',*,*,#5243,.F.);
#6486=ORIENTED_EDGE('',*,*,#5245,.F.);
#6487=ORIENTED_EDGE('',*,*,#5246,.T.);
#6488=ORIENTED_EDGE('',*,*,#5247,.F.);
#6489=ORIENTED_EDGE('',*,*,#5246,.F.);
#6490=ORIENTED_EDGE('',*,*,#5248,.F.);
#6491=ORIENTED_EDGE('',*,*,#5249,.T.);
#6492=ORIENTED_EDGE('',*,*,#5250,.F.);
#6493=ORIENTED_EDGE('',*,*,#5249,.F.);
#6494=ORIENTED_EDGE('',*,*,#5251,.F.);
#6495=ORIENTED_EDGE('',*,*,#5252,.T.);
#6496=ORIENTED_EDGE('',*,*,#5253,.F.);
#6497=ORIENTED_EDGE('',*,*,#5252,.F.);
#6498=ORIENTED_EDGE('',*,*,#5254,.F.);
#6499=ORIENTED_EDGE('',*,*,#5255,.T.);
#6500=ORIENTED_EDGE('',*,*,#5256,.F.);
#6501=ORIENTED_EDGE('',*,*,#5255,.F.);
#6502=ORIENTED_EDGE('',*,*,#5257,.F.);
#6503=ORIENTED_EDGE('',*,*,#5258,.T.);
#6504=ORIENTED_EDGE('',*,*,#5259,.F.);
#6505=ORIENTED_EDGE('',*,*,#5258,.F.);
#6506=ORIENTED_EDGE('',*,*,#5260,.F.);
#6507=ORIENTED_EDGE('',*,*,#5261,.T.);
#6508=ORIENTED_EDGE('',*,*,#5262,.F.);
#6509=ORIENTED_EDGE('',*,*,#5261,.F.);
#6510=ORIENTED_EDGE('',*,*,#5263,.F.);
#6511=ORIENTED_EDGE('',*,*,#5264,.T.);
#6512=ORIENTED_EDGE('',*,*,#5265,.F.);
#6513=ORIENTED_EDGE('',*,*,#5264,.F.);
#6514=ORIENTED_EDGE('',*,*,#5266,.F.);
#6515=ORIENTED_EDGE('',*,*,#5267,.T.);
#6516=ORIENTED_EDGE('',*,*,#5268,.F.);
#6517=ORIENTED_EDGE('',*,*,#5267,.F.);
#6518=ORIENTED_EDGE('',*,*,#5269,.F.);
#6519=ORIENTED_EDGE('',*,*,#5270,.T.);
#6520=ORIENTED_EDGE('',*,*,#5271,.F.);
#6521=ORIENTED_EDGE('',*,*,#5270,.F.);
#6522=ORIENTED_EDGE('',*,*,#5272,.T.);
#6523=ORIENTED_EDGE('',*,*,#5273,.T.);
#6524=ORIENTED_EDGE('',*,*,#5274,.F.);
#6525=ORIENTED_EDGE('',*,*,#5275,.F.);
#6526=ORIENTED_EDGE('',*,*,#5276,.T.);
#6527=ORIENTED_EDGE('',*,*,#5275,.T.);
#6528=ORIENTED_EDGE('',*,*,#5277,.F.);
#6529=ORIENTED_EDGE('',*,*,#5278,.F.);
#6530=ORIENTED_EDGE('',*,*,#5279,.T.);
#6531=ORIENTED_EDGE('',*,*,#5278,.T.);
#6532=ORIENTED_EDGE('',*,*,#5280,.F.);
#6533=ORIENTED_EDGE('',*,*,#5281,.F.);
#6534=ORIENTED_EDGE('',*,*,#5282,.T.);
#6535=ORIENTED_EDGE('',*,*,#5281,.T.);
#6536=ORIENTED_EDGE('',*,*,#5283,.F.);
#6537=ORIENTED_EDGE('',*,*,#5273,.F.);
#6538=ORIENTED_EDGE('',*,*,#5283,.T.);
#6539=ORIENTED_EDGE('',*,*,#5280,.T.);
#6540=ORIENTED_EDGE('',*,*,#5277,.T.);
#6541=ORIENTED_EDGE('',*,*,#5274,.T.);
#6542=ORIENTED_EDGE('',*,*,#5223,.T.);
#6543=ORIENTED_EDGE('',*,*,#5232,.T.);
#6544=ORIENTED_EDGE('',*,*,#5235,.T.);
#6545=ORIENTED_EDGE('',*,*,#5244,.T.);
#6546=ORIENTED_EDGE('',*,*,#5247,.T.);
#6547=ORIENTED_EDGE('',*,*,#5271,.T.);
#6548=ORIENTED_EDGE('',*,*,#5268,.T.);
#6549=ORIENTED_EDGE('',*,*,#5265,.T.);
#6550=ORIENTED_EDGE('',*,*,#5262,.T.);
#6551=ORIENTED_EDGE('',*,*,#5259,.T.);
#6552=ORIENTED_EDGE('',*,*,#5256,.T.);
#6553=ORIENTED_EDGE('',*,*,#5253,.T.);
#6554=ORIENTED_EDGE('',*,*,#5250,.T.);
#6555=ORIENTED_EDGE('',*,*,#5241,.T.);
#6556=ORIENTED_EDGE('',*,*,#5238,.T.);
#6557=ORIENTED_EDGE('',*,*,#5229,.T.);
#6558=ORIENTED_EDGE('',*,*,#5226,.T.);
#6559=ORIENTED_EDGE('',*,*,#5220,.T.);
#6560=ORIENTED_EDGE('',*,*,#5282,.F.);
#6561=ORIENTED_EDGE('',*,*,#5272,.F.);
#6562=ORIENTED_EDGE('',*,*,#5276,.F.);
#6563=ORIENTED_EDGE('',*,*,#5279,.F.);
#6564=ORIENTED_EDGE('',*,*,#5221,.T.);
#6565=ORIENTED_EDGE('',*,*,#5230,.T.);
#6566=ORIENTED_EDGE('',*,*,#5233,.T.);
#6567=ORIENTED_EDGE('',*,*,#5242,.T.);
#6568=ORIENTED_EDGE('',*,*,#5245,.T.);
#6569=ORIENTED_EDGE('',*,*,#5269,.T.);
#6570=ORIENTED_EDGE('',*,*,#5266,.T.);
#6571=ORIENTED_EDGE('',*,*,#5263,.T.);
#6572=ORIENTED_EDGE('',*,*,#5260,.T.);
#6573=ORIENTED_EDGE('',*,*,#5257,.T.);
#6574=ORIENTED_EDGE('',*,*,#5254,.T.);
#6575=ORIENTED_EDGE('',*,*,#5251,.T.);
#6576=ORIENTED_EDGE('',*,*,#5248,.T.);
#6577=ORIENTED_EDGE('',*,*,#5239,.T.);
#6578=ORIENTED_EDGE('',*,*,#5236,.T.);
#6579=ORIENTED_EDGE('',*,*,#5227,.T.);
#6580=ORIENTED_EDGE('',*,*,#5224,.T.);
#6581=ORIENTED_EDGE('',*,*,#5218,.T.);
#6582=ORIENTED_EDGE('',*,*,#5284,.F.);
#6583=ORIENTED_EDGE('',*,*,#5285,.T.);
#6584=ORIENTED_EDGE('',*,*,#5286,.F.);
#6585=ORIENTED_EDGE('',*,*,#5285,.F.);
#6586=ORIENTED_EDGE('',*,*,#5284,.T.);
#6587=ORIENTED_EDGE('',*,*,#5287,.F.);
#6588=ORIENTED_EDGE('',*,*,#5288,.T.);
#6589=ORIENTED_EDGE('',*,*,#5289,.F.);
#6590=ORIENTED_EDGE('',*,*,#5288,.F.);
#6591=ORIENTED_EDGE('',*,*,#5287,.T.);
#6592=ORIENTED_EDGE('',*,*,#5290,.F.);
#6593=ORIENTED_EDGE('',*,*,#5291,.T.);
#6594=ORIENTED_EDGE('',*,*,#5292,.T.);
#6595=ORIENTED_EDGE('',*,*,#5291,.F.);
#6596=ORIENTED_EDGE('',*,*,#5292,.F.);
#6597=ORIENTED_EDGE('',*,*,#5293,.F.);
#6598=ORIENTED_EDGE('',*,*,#5294,.T.);
#6599=ORIENTED_EDGE('',*,*,#5295,.T.);
#6600=ORIENTED_EDGE('',*,*,#5294,.F.);
#6601=ORIENTED_EDGE('',*,*,#5295,.F.);
#6602=ORIENTED_EDGE('',*,*,#5296,.T.);
#6603=ORIENTED_EDGE('',*,*,#5297,.T.);
#6604=ORIENTED_EDGE('',*,*,#5298,.F.);
#6605=ORIENTED_EDGE('',*,*,#5299,.F.);
#6606=ORIENTED_EDGE('',*,*,#5300,.T.);
#6607=ORIENTED_EDGE('',*,*,#5299,.T.);
#6608=ORIENTED_EDGE('',*,*,#5301,.F.);
#6609=ORIENTED_EDGE('',*,*,#5302,.F.);
#6610=ORIENTED_EDGE('',*,*,#5303,.T.);
#6611=ORIENTED_EDGE('',*,*,#5302,.T.);
#6612=ORIENTED_EDGE('',*,*,#5304,.F.);
#6613=ORIENTED_EDGE('',*,*,#5305,.F.);
#6614=ORIENTED_EDGE('',*,*,#5306,.T.);
#6615=ORIENTED_EDGE('',*,*,#5305,.T.);
#6616=ORIENTED_EDGE('',*,*,#5307,.F.);
#6617=ORIENTED_EDGE('',*,*,#5297,.F.);
#6618=ORIENTED_EDGE('',*,*,#5307,.T.);
#6619=ORIENTED_EDGE('',*,*,#5304,.T.);
#6620=ORIENTED_EDGE('',*,*,#5301,.T.);
#6621=ORIENTED_EDGE('',*,*,#5298,.T.);
#6622=ORIENTED_EDGE('',*,*,#5286,.T.);
#6623=ORIENTED_EDGE('',*,*,#5289,.T.);
#6624=ORIENTED_EDGE('',*,*,#5306,.F.);
#6625=ORIENTED_EDGE('',*,*,#5296,.F.);
#6626=ORIENTED_EDGE('',*,*,#5300,.F.);
#6627=ORIENTED_EDGE('',*,*,#5303,.F.);
#6628=ORIENTED_EDGE('',*,*,#5290,.T.);
#6629=ORIENTED_EDGE('',*,*,#5293,.T.);
#6630=ORIENTED_EDGE('',*,*,#5308,.F.);
#6631=ORIENTED_EDGE('',*,*,#5309,.T.);
#6632=ORIENTED_EDGE('',*,*,#5310,.F.);
#6633=ORIENTED_EDGE('',*,*,#5309,.F.);
#6634=ORIENTED_EDGE('',*,*,#5308,.T.);
#6635=ORIENTED_EDGE('',*,*,#5311,.F.);
#6636=ORIENTED_EDGE('',*,*,#5312,.T.);
#6637=ORIENTED_EDGE('',*,*,#5313,.F.);
#6638=ORIENTED_EDGE('',*,*,#5312,.F.);
#6639=ORIENTED_EDGE('',*,*,#5311,.T.);
#6640=ORIENTED_EDGE('',*,*,#5314,.F.);
#6641=ORIENTED_EDGE('',*,*,#5315,.T.);
#6642=ORIENTED_EDGE('',*,*,#5316,.T.);
#6643=ORIENTED_EDGE('',*,*,#5315,.F.);
#6644=ORIENTED_EDGE('',*,*,#5316,.F.);
#6645=ORIENTED_EDGE('',*,*,#5317,.F.);
#6646=ORIENTED_EDGE('',*,*,#5318,.T.);
#6647=ORIENTED_EDGE('',*,*,#5319,.T.);
#6648=ORIENTED_EDGE('',*,*,#5318,.F.);
#6649=ORIENTED_EDGE('',*,*,#5319,.F.);
#6650=ORIENTED_EDGE('',*,*,#5320,.T.);
#6651=ORIENTED_EDGE('',*,*,#5321,.T.);
#6652=ORIENTED_EDGE('',*,*,#5322,.F.);
#6653=ORIENTED_EDGE('',*,*,#5323,.F.);
#6654=ORIENTED_EDGE('',*,*,#5324,.T.);
#6655=ORIENTED_EDGE('',*,*,#5323,.T.);
#6656=ORIENTED_EDGE('',*,*,#5325,.F.);
#6657=ORIENTED_EDGE('',*,*,#5326,.F.);
#6658=ORIENTED_EDGE('',*,*,#5327,.T.);
#6659=ORIENTED_EDGE('',*,*,#5326,.T.);
#6660=ORIENTED_EDGE('',*,*,#5328,.F.);
#6661=ORIENTED_EDGE('',*,*,#5329,.F.);
#6662=ORIENTED_EDGE('',*,*,#5330,.T.);
#6663=ORIENTED_EDGE('',*,*,#5329,.T.);
#6664=ORIENTED_EDGE('',*,*,#5331,.F.);
#6665=ORIENTED_EDGE('',*,*,#5321,.F.);
#6666=ORIENTED_EDGE('',*,*,#5331,.T.);
#6667=ORIENTED_EDGE('',*,*,#5328,.T.);
#6668=ORIENTED_EDGE('',*,*,#5325,.T.);
#6669=ORIENTED_EDGE('',*,*,#5322,.T.);
#6670=ORIENTED_EDGE('',*,*,#5310,.T.);
#6671=ORIENTED_EDGE('',*,*,#5313,.T.);
#6672=ORIENTED_EDGE('',*,*,#5330,.F.);
#6673=ORIENTED_EDGE('',*,*,#5320,.F.);
#6674=ORIENTED_EDGE('',*,*,#5324,.F.);
#6675=ORIENTED_EDGE('',*,*,#5327,.F.);
#6676=ORIENTED_EDGE('',*,*,#5314,.T.);
#6677=ORIENTED_EDGE('',*,*,#5317,.T.);
#6678=ORIENTED_EDGE('',*,*,#5332,.F.);
#6679=ORIENTED_EDGE('',*,*,#5333,.T.);
#6680=ORIENTED_EDGE('',*,*,#5334,.T.);
#6681=ORIENTED_EDGE('',*,*,#5333,.F.);
#6682=ORIENTED_EDGE('',*,*,#5334,.F.);
#6683=ORIENTED_EDGE('',*,*,#5335,.F.);
#6684=ORIENTED_EDGE('',*,*,#5336,.T.);
#6685=ORIENTED_EDGE('',*,*,#5337,.T.);
#6686=ORIENTED_EDGE('',*,*,#5336,.F.);
#6687=ORIENTED_EDGE('',*,*,#5337,.F.);
#6688=ORIENTED_EDGE('',*,*,#5338,.F.);
#6689=ORIENTED_EDGE('',*,*,#5339,.T.);
#6690=ORIENTED_EDGE('',*,*,#5340,.F.);
#6691=ORIENTED_EDGE('',*,*,#5339,.F.);
#6692=ORIENTED_EDGE('',*,*,#5341,.F.);
#6693=ORIENTED_EDGE('',*,*,#5342,.T.);
#6694=ORIENTED_EDGE('',*,*,#5343,.F.);
#6695=ORIENTED_EDGE('',*,*,#5342,.F.);
#6696=ORIENTED_EDGE('',*,*,#5344,.T.);
#6697=ORIENTED_EDGE('',*,*,#5345,.T.);
#6698=ORIENTED_EDGE('',*,*,#5346,.F.);
#6699=ORIENTED_EDGE('',*,*,#5347,.F.);
#6700=ORIENTED_EDGE('',*,*,#5340,.T.);
#6701=ORIENTED_EDGE('',*,*,#5343,.T.);
#6702=ORIENTED_EDGE('',*,*,#5348,.T.);
#6703=ORIENTED_EDGE('',*,*,#5347,.T.);
#6704=ORIENTED_EDGE('',*,*,#5349,.F.);
#6705=ORIENTED_EDGE('',*,*,#5350,.F.);
#6706=ORIENTED_EDGE('',*,*,#5351,.T.);
#6707=ORIENTED_EDGE('',*,*,#5350,.T.);
#6708=ORIENTED_EDGE('',*,*,#5352,.F.);
#6709=ORIENTED_EDGE('',*,*,#5353,.F.);
#6710=ORIENTED_EDGE('',*,*,#5338,.T.);
#6711=ORIENTED_EDGE('',*,*,#5341,.T.);
#6712=ORIENTED_EDGE('',*,*,#5354,.T.);
#6713=ORIENTED_EDGE('',*,*,#5353,.T.);
#6714=ORIENTED_EDGE('',*,*,#5355,.F.);
#6715=ORIENTED_EDGE('',*,*,#5345,.F.);
#6716=ORIENTED_EDGE('',*,*,#5355,.T.);
#6717=ORIENTED_EDGE('',*,*,#5352,.T.);
#6718=ORIENTED_EDGE('',*,*,#5349,.T.);
#6719=ORIENTED_EDGE('',*,*,#5346,.T.);
#6720=ORIENTED_EDGE('',*,*,#5354,.F.);
#6721=ORIENTED_EDGE('',*,*,#5344,.F.);
#6722=ORIENTED_EDGE('',*,*,#5348,.F.);
#6723=ORIENTED_EDGE('',*,*,#5351,.F.);
#6724=ORIENTED_EDGE('',*,*,#5332,.T.);
#6725=ORIENTED_EDGE('',*,*,#5335,.T.);
#6726=ORIENTED_EDGE('',*,*,#5356,.F.);
#6727=ORIENTED_EDGE('',*,*,#5357,.T.);
#6728=ORIENTED_EDGE('',*,*,#5358,.F.);
#6729=ORIENTED_EDGE('',*,*,#5357,.F.);
#6730=ORIENTED_EDGE('',*,*,#5359,.F.);
#6731=ORIENTED_EDGE('',*,*,#5360,.T.);
#6732=ORIENTED_EDGE('',*,*,#5361,.F.);
#6733=ORIENTED_EDGE('',*,*,#5360,.F.);
#6734=ORIENTED_EDGE('',*,*,#5362,.F.);
#6735=ORIENTED_EDGE('',*,*,#5363,.T.);
#6736=ORIENTED_EDGE('',*,*,#5364,.T.);
#6737=ORIENTED_EDGE('',*,*,#5365,.F.);
#6738=ORIENTED_EDGE('',*,*,#5366,.F.);
#6739=ORIENTED_EDGE('',*,*,#5367,.F.);
#6740=ORIENTED_EDGE('',*,*,#5368,.T.);
#6741=ORIENTED_EDGE('',*,*,#5363,.F.);
#6742=ORIENTED_EDGE('',*,*,#5369,.F.);
#6743=ORIENTED_EDGE('',*,*,#5364,.F.);
#6744=ORIENTED_EDGE('',*,*,#5368,.F.);
#6745=ORIENTED_EDGE('',*,*,#5370,.F.);
#6746=ORIENTED_EDGE('',*,*,#5371,.T.);
#6747=ORIENTED_EDGE('',*,*,#5372,.T.);
#6748=ORIENTED_EDGE('',*,*,#5373,.F.);
#6749=ORIENTED_EDGE('',*,*,#5374,.F.);
#6750=ORIENTED_EDGE('',*,*,#5375,.F.);
#6751=ORIENTED_EDGE('',*,*,#5376,.T.);
#6752=ORIENTED_EDGE('',*,*,#5371,.F.);
#6753=ORIENTED_EDGE('',*,*,#5377,.F.);
#6754=ORIENTED_EDGE('',*,*,#5372,.F.);
#6755=ORIENTED_EDGE('',*,*,#5376,.F.);
#6756=ORIENTED_EDGE('',*,*,#5366,.T.);
#6757=ORIENTED_EDGE('',*,*,#5378,.T.);
#6758=ORIENTED_EDGE('',*,*,#5374,.T.);
#6759=ORIENTED_EDGE('',*,*,#5379,.T.);
#6760=ORIENTED_EDGE('',*,*,#5380,.F.);
#6761=ORIENTED_EDGE('',*,*,#5381,.T.);
#6762=ORIENTED_EDGE('',*,*,#5382,.T.);
#6763=ORIENTED_EDGE('',*,*,#5383,.T.);
#6764=ORIENTED_EDGE('',*,*,#5367,.T.);
#6765=ORIENTED_EDGE('',*,*,#5383,.F.);
#6766=ORIENTED_EDGE('',*,*,#5384,.T.);
#6767=ORIENTED_EDGE('',*,*,#5385,.F.);
#6768=ORIENTED_EDGE('',*,*,#5386,.F.);
#6769=ORIENTED_EDGE('',*,*,#5379,.F.);
#6770=ORIENTED_EDGE('',*,*,#5373,.T.);
#6771=ORIENTED_EDGE('',*,*,#5377,.T.);
#6772=ORIENTED_EDGE('',*,*,#5375,.T.);
#6773=ORIENTED_EDGE('',*,*,#5378,.F.);
#6774=ORIENTED_EDGE('',*,*,#5365,.T.);
#6775=ORIENTED_EDGE('',*,*,#5369,.T.);
#6776=ORIENTED_EDGE('',*,*,#5356,.T.);
#6777=ORIENTED_EDGE('',*,*,#5359,.T.);
#6778=ORIENTED_EDGE('',*,*,#5387,.T.);
#6779=ORIENTED_EDGE('',*,*,#5388,.T.);
#6780=ORIENTED_EDGE('',*,*,#5385,.T.);
#6781=ORIENTED_EDGE('',*,*,#5389,.T.);
#6782=ORIENTED_EDGE('',*,*,#5390,.F.);
#6783=ORIENTED_EDGE('',*,*,#5391,.T.);
#6784=ORIENTED_EDGE('',*,*,#5380,.T.);
#6785=ORIENTED_EDGE('',*,*,#5386,.T.);
#6786=ORIENTED_EDGE('',*,*,#5388,.F.);
#6787=ORIENTED_EDGE('',*,*,#5392,.F.);
#6788=ORIENTED_EDGE('',*,*,#5393,.F.);
#6789=ORIENTED_EDGE('',*,*,#5394,.T.);
#6790=ORIENTED_EDGE('',*,*,#5390,.T.);
#6791=ORIENTED_EDGE('',*,*,#5395,.F.);
#6792=ORIENTED_EDGE('',*,*,#5362,.T.);
#6793=ORIENTED_EDGE('',*,*,#5370,.T.);
#6794=ORIENTED_EDGE('',*,*,#5382,.F.);
#6795=ORIENTED_EDGE('',*,*,#5396,.T.);
#6796=ORIENTED_EDGE('',*,*,#5393,.T.);
#6797=ORIENTED_EDGE('',*,*,#5397,.T.);
#6798=ORIENTED_EDGE('',*,*,#5389,.F.);
#6799=ORIENTED_EDGE('',*,*,#5384,.F.);
#6800=ORIENTED_EDGE('',*,*,#5397,.F.);
#6801=ORIENTED_EDGE('',*,*,#5395,.T.);
#6802=ORIENTED_EDGE('',*,*,#5392,.T.);
#6803=ORIENTED_EDGE('',*,*,#5387,.F.);
#6804=ORIENTED_EDGE('',*,*,#5358,.T.);
#6805=ORIENTED_EDGE('',*,*,#5361,.T.);
#6806=ORIENTED_EDGE('',*,*,#5396,.F.);
#6807=ORIENTED_EDGE('',*,*,#5381,.F.);
#6808=ORIENTED_EDGE('',*,*,#5391,.F.);
#6809=ORIENTED_EDGE('',*,*,#5394,.F.);
#6810=ORIENTED_EDGE('',*,*,#5398,.F.);
#6811=ORIENTED_EDGE('',*,*,#5399,.T.);
#6812=ORIENTED_EDGE('',*,*,#5400,.T.);
#6813=ORIENTED_EDGE('',*,*,#5399,.F.);
#6814=ORIENTED_EDGE('',*,*,#5401,.F.);
#6815=ORIENTED_EDGE('',*,*,#5402,.T.);
#6816=ORIENTED_EDGE('',*,*,#5403,.T.);
#6817=ORIENTED_EDGE('',*,*,#5402,.F.);
#6818=ORIENTED_EDGE('',*,*,#5401,.T.);
#6819=ORIENTED_EDGE('',*,*,#5398,.T.);
#6820=ORIENTED_EDGE('',*,*,#5403,.F.);
#6821=ORIENTED_EDGE('',*,*,#5400,.F.);
#6822=ORIENTED_EDGE('',*,*,#5404,.T.);
#6823=ORIENTED_EDGE('',*,*,#5405,.T.);
#6824=ORIENTED_EDGE('',*,*,#5406,.F.);
#6825=ORIENTED_EDGE('',*,*,#5405,.F.);
#6826=ORIENTED_EDGE('',*,*,#5406,.T.);
#6827=ORIENTED_EDGE('',*,*,#5404,.F.);
#6828=ORIENTED_EDGE('',*,*,#5407,.F.);
#6829=ORIENTED_EDGE('',*,*,#5408,.T.);
#6830=ORIENTED_EDGE('',*,*,#5409,.T.);
#6831=ORIENTED_EDGE('',*,*,#5408,.F.);
#6832=ORIENTED_EDGE('',*,*,#5409,.F.);
#6833=ORIENTED_EDGE('',*,*,#5410,.F.);
#6834=ORIENTED_EDGE('',*,*,#5411,.T.);
#6835=ORIENTED_EDGE('',*,*,#5412,.T.);
#6836=ORIENTED_EDGE('',*,*,#5411,.F.);
#6837=ORIENTED_EDGE('',*,*,#5412,.F.);
#6838=ORIENTED_EDGE('',*,*,#5413,.F.);
#6839=ORIENTED_EDGE('',*,*,#5414,.T.);
#6840=ORIENTED_EDGE('',*,*,#5415,.F.);
#6841=ORIENTED_EDGE('',*,*,#5414,.F.);
#6842=ORIENTED_EDGE('',*,*,#5416,.F.);
#6843=ORIENTED_EDGE('',*,*,#5417,.T.);
#6844=ORIENTED_EDGE('',*,*,#5418,.F.);
#6845=ORIENTED_EDGE('',*,*,#5417,.F.);
#6846=ORIENTED_EDGE('',*,*,#5419,.T.);
#6847=ORIENTED_EDGE('',*,*,#5420,.T.);
#6848=ORIENTED_EDGE('',*,*,#5421,.F.);
#6849=ORIENTED_EDGE('',*,*,#5422,.F.);
#6850=ORIENTED_EDGE('',*,*,#5415,.T.);
#6851=ORIENTED_EDGE('',*,*,#5418,.T.);
#6852=ORIENTED_EDGE('',*,*,#5423,.T.);
#6853=ORIENTED_EDGE('',*,*,#5422,.T.);
#6854=ORIENTED_EDGE('',*,*,#5424,.F.);
#6855=ORIENTED_EDGE('',*,*,#5425,.F.);
#6856=ORIENTED_EDGE('',*,*,#5426,.T.);
#6857=ORIENTED_EDGE('',*,*,#5425,.T.);
#6858=ORIENTED_EDGE('',*,*,#5427,.F.);
#6859=ORIENTED_EDGE('',*,*,#5428,.F.);
#6860=ORIENTED_EDGE('',*,*,#5413,.T.);
#6861=ORIENTED_EDGE('',*,*,#5416,.T.);
#6862=ORIENTED_EDGE('',*,*,#5429,.T.);
#6863=ORIENTED_EDGE('',*,*,#5428,.T.);
#6864=ORIENTED_EDGE('',*,*,#5430,.F.);
#6865=ORIENTED_EDGE('',*,*,#5420,.F.);
#6866=ORIENTED_EDGE('',*,*,#5430,.T.);
#6867=ORIENTED_EDGE('',*,*,#5427,.T.);
#6868=ORIENTED_EDGE('',*,*,#5424,.T.);
#6869=ORIENTED_EDGE('',*,*,#5421,.T.);
#6870=ORIENTED_EDGE('',*,*,#5429,.F.);
#6871=ORIENTED_EDGE('',*,*,#5419,.F.);
#6872=ORIENTED_EDGE('',*,*,#5423,.F.);
#6873=ORIENTED_EDGE('',*,*,#5426,.F.);
#6874=ORIENTED_EDGE('',*,*,#5407,.T.);
#6875=ORIENTED_EDGE('',*,*,#5410,.T.);
#6876=ORIENTED_EDGE('',*,*,#5431,.F.);
#6877=ORIENTED_EDGE('',*,*,#5432,.T.);
#6878=ORIENTED_EDGE('',*,*,#5433,.F.);
#6879=ORIENTED_EDGE('',*,*,#5432,.F.);
#6880=ORIENTED_EDGE('',*,*,#5434,.F.);
#6881=ORIENTED_EDGE('',*,*,#5435,.T.);
#6882=ORIENTED_EDGE('',*,*,#5436,.F.);
#6883=ORIENTED_EDGE('',*,*,#5435,.F.);
#6884=ORIENTED_EDGE('',*,*,#5437,.F.);
#6885=ORIENTED_EDGE('',*,*,#5438,.T.);
#6886=ORIENTED_EDGE('',*,*,#5439,.T.);
#6887=ORIENTED_EDGE('',*,*,#5440,.F.);
#6888=ORIENTED_EDGE('',*,*,#5441,.F.);
#6889=ORIENTED_EDGE('',*,*,#5442,.F.);
#6890=ORIENTED_EDGE('',*,*,#5443,.T.);
#6891=ORIENTED_EDGE('',*,*,#5438,.F.);
#6892=ORIENTED_EDGE('',*,*,#5444,.F.);
#6893=ORIENTED_EDGE('',*,*,#5439,.F.);
#6894=ORIENTED_EDGE('',*,*,#5443,.F.);
#6895=ORIENTED_EDGE('',*,*,#5445,.F.);
#6896=ORIENTED_EDGE('',*,*,#5446,.T.);
#6897=ORIENTED_EDGE('',*,*,#5447,.T.);
#6898=ORIENTED_EDGE('',*,*,#5448,.F.);
#6899=ORIENTED_EDGE('',*,*,#5449,.F.);
#6900=ORIENTED_EDGE('',*,*,#5450,.F.);
#6901=ORIENTED_EDGE('',*,*,#5451,.T.);
#6902=ORIENTED_EDGE('',*,*,#5446,.F.);
#6903=ORIENTED_EDGE('',*,*,#5452,.F.);
#6904=ORIENTED_EDGE('',*,*,#5447,.F.);
#6905=ORIENTED_EDGE('',*,*,#5451,.F.);
#6906=ORIENTED_EDGE('',*,*,#5441,.T.);
#6907=ORIENTED_EDGE('',*,*,#5453,.T.);
#6908=ORIENTED_EDGE('',*,*,#5449,.T.);
#6909=ORIENTED_EDGE('',*,*,#5454,.T.);
#6910=ORIENTED_EDGE('',*,*,#5455,.F.);
#6911=ORIENTED_EDGE('',*,*,#5456,.T.);
#6912=ORIENTED_EDGE('',*,*,#5457,.T.);
#6913=ORIENTED_EDGE('',*,*,#5458,.T.);
#6914=ORIENTED_EDGE('',*,*,#5442,.T.);
#6915=ORIENTED_EDGE('',*,*,#5458,.F.);
#6916=ORIENTED_EDGE('',*,*,#5459,.T.);
#6917=ORIENTED_EDGE('',*,*,#5460,.F.);
#6918=ORIENTED_EDGE('',*,*,#5461,.F.);
#6919=ORIENTED_EDGE('',*,*,#5454,.F.);
#6920=ORIENTED_EDGE('',*,*,#5448,.T.);
#6921=ORIENTED_EDGE('',*,*,#5452,.T.);
#6922=ORIENTED_EDGE('',*,*,#5450,.T.);
#6923=ORIENTED_EDGE('',*,*,#5453,.F.);
#6924=ORIENTED_EDGE('',*,*,#5440,.T.);
#6925=ORIENTED_EDGE('',*,*,#5444,.T.);
#6926=ORIENTED_EDGE('',*,*,#5431,.T.);
#6927=ORIENTED_EDGE('',*,*,#5434,.T.);
#6928=ORIENTED_EDGE('',*,*,#5462,.T.);
#6929=ORIENTED_EDGE('',*,*,#5463,.T.);
#6930=ORIENTED_EDGE('',*,*,#5460,.T.);
#6931=ORIENTED_EDGE('',*,*,#5464,.T.);
#6932=ORIENTED_EDGE('',*,*,#5465,.F.);
#6933=ORIENTED_EDGE('',*,*,#5466,.T.);
#6934=ORIENTED_EDGE('',*,*,#5455,.T.);
#6935=ORIENTED_EDGE('',*,*,#5461,.T.);
#6936=ORIENTED_EDGE('',*,*,#5463,.F.);
#6937=ORIENTED_EDGE('',*,*,#5467,.F.);
#6938=ORIENTED_EDGE('',*,*,#5468,.F.);
#6939=ORIENTED_EDGE('',*,*,#5469,.T.);
#6940=ORIENTED_EDGE('',*,*,#5465,.T.);
#6941=ORIENTED_EDGE('',*,*,#5470,.F.);
#6942=ORIENTED_EDGE('',*,*,#5437,.T.);
#6943=ORIENTED_EDGE('',*,*,#5445,.T.);
#6944=ORIENTED_EDGE('',*,*,#5457,.F.);
#6945=ORIENTED_EDGE('',*,*,#5471,.T.);
#6946=ORIENTED_EDGE('',*,*,#5468,.T.);
#6947=ORIENTED_EDGE('',*,*,#5472,.T.);
#6948=ORIENTED_EDGE('',*,*,#5464,.F.);
#6949=ORIENTED_EDGE('',*,*,#5459,.F.);
#6950=ORIENTED_EDGE('',*,*,#5472,.F.);
#6951=ORIENTED_EDGE('',*,*,#5470,.T.);
#6952=ORIENTED_EDGE('',*,*,#5467,.T.);
#6953=ORIENTED_EDGE('',*,*,#5462,.F.);
#6954=ORIENTED_EDGE('',*,*,#5433,.T.);
#6955=ORIENTED_EDGE('',*,*,#5436,.T.);
#6956=ORIENTED_EDGE('',*,*,#5471,.F.);
#6957=ORIENTED_EDGE('',*,*,#5456,.F.);
#6958=ORIENTED_EDGE('',*,*,#5466,.F.);
#6959=ORIENTED_EDGE('',*,*,#5469,.F.);
#6960=ORIENTED_EDGE('',*,*,#5473,.F.);
#6961=ORIENTED_EDGE('',*,*,#5474,.T.);
#6962=ORIENTED_EDGE('',*,*,#5475,.T.);
#6963=ORIENTED_EDGE('',*,*,#5474,.F.);
#6964=ORIENTED_EDGE('',*,*,#5476,.F.);
#6965=ORIENTED_EDGE('',*,*,#5477,.T.);
#6966=ORIENTED_EDGE('',*,*,#5478,.T.);
#6967=ORIENTED_EDGE('',*,*,#5477,.F.);
#6968=ORIENTED_EDGE('',*,*,#5476,.T.);
#6969=ORIENTED_EDGE('',*,*,#5473,.T.);
#6970=ORIENTED_EDGE('',*,*,#5478,.F.);
#6971=ORIENTED_EDGE('',*,*,#5475,.F.);
#6972=ORIENTED_EDGE('',*,*,#5479,.T.);
#6973=ORIENTED_EDGE('',*,*,#5480,.T.);
#6974=ORIENTED_EDGE('',*,*,#5481,.F.);
#6975=ORIENTED_EDGE('',*,*,#5480,.F.);
#6976=ORIENTED_EDGE('',*,*,#5481,.T.);
#6977=ORIENTED_EDGE('',*,*,#5479,.F.);
#6978=ORIENTED_EDGE('',*,*,#5482,.F.);
#6979=ORIENTED_EDGE('',*,*,#5483,.T.);
#6980=ORIENTED_EDGE('',*,*,#5484,.T.);
#6981=ORIENTED_EDGE('',*,*,#5483,.F.);
#6982=ORIENTED_EDGE('',*,*,#5484,.F.);
#6983=ORIENTED_EDGE('',*,*,#5485,.F.);
#6984=ORIENTED_EDGE('',*,*,#5486,.T.);
#6985=ORIENTED_EDGE('',*,*,#5487,.T.);
#6986=ORIENTED_EDGE('',*,*,#5486,.F.);
#6987=ORIENTED_EDGE('',*,*,#5487,.F.);
#6988=ORIENTED_EDGE('',*,*,#5488,.F.);
#6989=ORIENTED_EDGE('',*,*,#5489,.T.);
#6990=ORIENTED_EDGE('',*,*,#5490,.F.);
#6991=ORIENTED_EDGE('',*,*,#5489,.F.);
#6992=ORIENTED_EDGE('',*,*,#5491,.F.);
#6993=ORIENTED_EDGE('',*,*,#5492,.T.);
#6994=ORIENTED_EDGE('',*,*,#5493,.F.);
#6995=ORIENTED_EDGE('',*,*,#5492,.F.);
#6996=ORIENTED_EDGE('',*,*,#5494,.T.);
#6997=ORIENTED_EDGE('',*,*,#5495,.T.);
#6998=ORIENTED_EDGE('',*,*,#5496,.F.);
#6999=ORIENTED_EDGE('',*,*,#5497,.F.);
#7000=ORIENTED_EDGE('',*,*,#5490,.T.);
#7001=ORIENTED_EDGE('',*,*,#5493,.T.);
#7002=ORIENTED_EDGE('',*,*,#5498,.T.);
#7003=ORIENTED_EDGE('',*,*,#5497,.T.);
#7004=ORIENTED_EDGE('',*,*,#5499,.F.);
#7005=ORIENTED_EDGE('',*,*,#5500,.F.);
#7006=ORIENTED_EDGE('',*,*,#5501,.T.);
#7007=ORIENTED_EDGE('',*,*,#5500,.T.);
#7008=ORIENTED_EDGE('',*,*,#5502,.F.);
#7009=ORIENTED_EDGE('',*,*,#5503,.F.);
#7010=ORIENTED_EDGE('',*,*,#5488,.T.);
#7011=ORIENTED_EDGE('',*,*,#5491,.T.);
#7012=ORIENTED_EDGE('',*,*,#5504,.T.);
#7013=ORIENTED_EDGE('',*,*,#5503,.T.);
#7014=ORIENTED_EDGE('',*,*,#5505,.F.);
#7015=ORIENTED_EDGE('',*,*,#5495,.F.);
#7016=ORIENTED_EDGE('',*,*,#5505,.T.);
#7017=ORIENTED_EDGE('',*,*,#5502,.T.);
#7018=ORIENTED_EDGE('',*,*,#5499,.T.);
#7019=ORIENTED_EDGE('',*,*,#5496,.T.);
#7020=ORIENTED_EDGE('',*,*,#5504,.F.);
#7021=ORIENTED_EDGE('',*,*,#5494,.F.);
#7022=ORIENTED_EDGE('',*,*,#5498,.F.);
#7023=ORIENTED_EDGE('',*,*,#5501,.F.);
#7024=ORIENTED_EDGE('',*,*,#5482,.T.);
#7025=ORIENTED_EDGE('',*,*,#5485,.T.);
#7026=ORIENTED_EDGE('',*,*,#5506,.F.);
#7027=ORIENTED_EDGE('',*,*,#5507,.T.);
#7028=ORIENTED_EDGE('',*,*,#5508,.F.);
#7029=ORIENTED_EDGE('',*,*,#5507,.F.);
#7030=ORIENTED_EDGE('',*,*,#5509,.F.);
#7031=ORIENTED_EDGE('',*,*,#5510,.T.);
#7032=ORIENTED_EDGE('',*,*,#5511,.F.);
#7033=ORIENTED_EDGE('',*,*,#5510,.F.);
#7034=ORIENTED_EDGE('',*,*,#5512,.F.);
#7035=ORIENTED_EDGE('',*,*,#5513,.T.);
#7036=ORIENTED_EDGE('',*,*,#5514,.T.);
#7037=ORIENTED_EDGE('',*,*,#5515,.F.);
#7038=ORIENTED_EDGE('',*,*,#5516,.F.);
#7039=ORIENTED_EDGE('',*,*,#5517,.F.);
#7040=ORIENTED_EDGE('',*,*,#5518,.T.);
#7041=ORIENTED_EDGE('',*,*,#5513,.F.);
#7042=ORIENTED_EDGE('',*,*,#5519,.F.);
#7043=ORIENTED_EDGE('',*,*,#5514,.F.);
#7044=ORIENTED_EDGE('',*,*,#5518,.F.);
#7045=ORIENTED_EDGE('',*,*,#5520,.F.);
#7046=ORIENTED_EDGE('',*,*,#5521,.T.);
#7047=ORIENTED_EDGE('',*,*,#5522,.T.);
#7048=ORIENTED_EDGE('',*,*,#5523,.F.);
#7049=ORIENTED_EDGE('',*,*,#5524,.F.);
#7050=ORIENTED_EDGE('',*,*,#5525,.F.);
#7051=ORIENTED_EDGE('',*,*,#5526,.T.);
#7052=ORIENTED_EDGE('',*,*,#5521,.F.);
#7053=ORIENTED_EDGE('',*,*,#5527,.F.);
#7054=ORIENTED_EDGE('',*,*,#5522,.F.);
#7055=ORIENTED_EDGE('',*,*,#5526,.F.);
#7056=ORIENTED_EDGE('',*,*,#5516,.T.);
#7057=ORIENTED_EDGE('',*,*,#5528,.T.);
#7058=ORIENTED_EDGE('',*,*,#5524,.T.);
#7059=ORIENTED_EDGE('',*,*,#5529,.T.);
#7060=ORIENTED_EDGE('',*,*,#5530,.F.);
#7061=ORIENTED_EDGE('',*,*,#5531,.T.);
#7062=ORIENTED_EDGE('',*,*,#5532,.T.);
#7063=ORIENTED_EDGE('',*,*,#5533,.T.);
#7064=ORIENTED_EDGE('',*,*,#5517,.T.);
#7065=ORIENTED_EDGE('',*,*,#5533,.F.);
#7066=ORIENTED_EDGE('',*,*,#5534,.T.);
#7067=ORIENTED_EDGE('',*,*,#5535,.F.);
#7068=ORIENTED_EDGE('',*,*,#5536,.F.);
#7069=ORIENTED_EDGE('',*,*,#5529,.F.);
#7070=ORIENTED_EDGE('',*,*,#5523,.T.);
#7071=ORIENTED_EDGE('',*,*,#5527,.T.);
#7072=ORIENTED_EDGE('',*,*,#5525,.T.);
#7073=ORIENTED_EDGE('',*,*,#5528,.F.);
#7074=ORIENTED_EDGE('',*,*,#5515,.T.);
#7075=ORIENTED_EDGE('',*,*,#5519,.T.);
#7076=ORIENTED_EDGE('',*,*,#5506,.T.);
#7077=ORIENTED_EDGE('',*,*,#5509,.T.);
#7078=ORIENTED_EDGE('',*,*,#5537,.T.);
#7079=ORIENTED_EDGE('',*,*,#5538,.T.);
#7080=ORIENTED_EDGE('',*,*,#5535,.T.);
#7081=ORIENTED_EDGE('',*,*,#5539,.T.);
#7082=ORIENTED_EDGE('',*,*,#5540,.F.);
#7083=ORIENTED_EDGE('',*,*,#5541,.T.);
#7084=ORIENTED_EDGE('',*,*,#5530,.T.);
#7085=ORIENTED_EDGE('',*,*,#5536,.T.);
#7086=ORIENTED_EDGE('',*,*,#5538,.F.);
#7087=ORIENTED_EDGE('',*,*,#5542,.F.);
#7088=ORIENTED_EDGE('',*,*,#5543,.F.);
#7089=ORIENTED_EDGE('',*,*,#5544,.T.);
#7090=ORIENTED_EDGE('',*,*,#5540,.T.);
#7091=ORIENTED_EDGE('',*,*,#5545,.F.);
#7092=ORIENTED_EDGE('',*,*,#5512,.T.);
#7093=ORIENTED_EDGE('',*,*,#5520,.T.);
#7094=ORIENTED_EDGE('',*,*,#5532,.F.);
#7095=ORIENTED_EDGE('',*,*,#5546,.T.);
#7096=ORIENTED_EDGE('',*,*,#5543,.T.);
#7097=ORIENTED_EDGE('',*,*,#5547,.T.);
#7098=ORIENTED_EDGE('',*,*,#5539,.F.);
#7099=ORIENTED_EDGE('',*,*,#5534,.F.);
#7100=ORIENTED_EDGE('',*,*,#5547,.F.);
#7101=ORIENTED_EDGE('',*,*,#5545,.T.);
#7102=ORIENTED_EDGE('',*,*,#5542,.T.);
#7103=ORIENTED_EDGE('',*,*,#5537,.F.);
#7104=ORIENTED_EDGE('',*,*,#5508,.T.);
#7105=ORIENTED_EDGE('',*,*,#5511,.T.);
#7106=ORIENTED_EDGE('',*,*,#5546,.F.);
#7107=ORIENTED_EDGE('',*,*,#5531,.F.);
#7108=ORIENTED_EDGE('',*,*,#5541,.F.);
#7109=ORIENTED_EDGE('',*,*,#5544,.F.);
#7110=ORIENTED_EDGE('',*,*,#5548,.F.);
#7111=ORIENTED_EDGE('',*,*,#5549,.T.);
#7112=ORIENTED_EDGE('',*,*,#5550,.T.);
#7113=ORIENTED_EDGE('',*,*,#5549,.F.);
#7114=ORIENTED_EDGE('',*,*,#5551,.F.);
#7115=ORIENTED_EDGE('',*,*,#5552,.T.);
#7116=ORIENTED_EDGE('',*,*,#5553,.T.);
#7117=ORIENTED_EDGE('',*,*,#5552,.F.);
#7118=ORIENTED_EDGE('',*,*,#5551,.T.);
#7119=ORIENTED_EDGE('',*,*,#5548,.T.);
#7120=ORIENTED_EDGE('',*,*,#5553,.F.);
#7121=ORIENTED_EDGE('',*,*,#5550,.F.);
#7122=ORIENTED_EDGE('',*,*,#5554,.T.);
#7123=ORIENTED_EDGE('',*,*,#5555,.T.);
#7124=ORIENTED_EDGE('',*,*,#5556,.F.);
#7125=ORIENTED_EDGE('',*,*,#5555,.F.);
#7126=ORIENTED_EDGE('',*,*,#5556,.T.);
#7127=ORIENTED_EDGE('',*,*,#5554,.F.);
#7128=ORIENTED_EDGE('',*,*,#5557,.F.);
#7129=ORIENTED_EDGE('',*,*,#5558,.T.);
#7130=ORIENTED_EDGE('',*,*,#5559,.T.);
#7131=ORIENTED_EDGE('',*,*,#5558,.F.);
#7132=ORIENTED_EDGE('',*,*,#5559,.F.);
#7133=ORIENTED_EDGE('',*,*,#5560,.F.);
#7134=ORIENTED_EDGE('',*,*,#5561,.T.);
#7135=ORIENTED_EDGE('',*,*,#5562,.T.);
#7136=ORIENTED_EDGE('',*,*,#5561,.F.);
#7137=ORIENTED_EDGE('',*,*,#5562,.F.);
#7138=ORIENTED_EDGE('',*,*,#5563,.F.);
#7139=ORIENTED_EDGE('',*,*,#5564,.T.);
#7140=ORIENTED_EDGE('',*,*,#5565,.F.);
#7141=ORIENTED_EDGE('',*,*,#5564,.F.);
#7142=ORIENTED_EDGE('',*,*,#5566,.F.);
#7143=ORIENTED_EDGE('',*,*,#5567,.T.);
#7144=ORIENTED_EDGE('',*,*,#5568,.F.);
#7145=ORIENTED_EDGE('',*,*,#5567,.F.);
#7146=ORIENTED_EDGE('',*,*,#5569,.T.);
#7147=ORIENTED_EDGE('',*,*,#5570,.T.);
#7148=ORIENTED_EDGE('',*,*,#5571,.F.);
#7149=ORIENTED_EDGE('',*,*,#5572,.F.);
#7150=ORIENTED_EDGE('',*,*,#5565,.T.);
#7151=ORIENTED_EDGE('',*,*,#5568,.T.);
#7152=ORIENTED_EDGE('',*,*,#5573,.T.);
#7153=ORIENTED_EDGE('',*,*,#5572,.T.);
#7154=ORIENTED_EDGE('',*,*,#5574,.F.);
#7155=ORIENTED_EDGE('',*,*,#5575,.F.);
#7156=ORIENTED_EDGE('',*,*,#5576,.T.);
#7157=ORIENTED_EDGE('',*,*,#5575,.T.);
#7158=ORIENTED_EDGE('',*,*,#5577,.F.);
#7159=ORIENTED_EDGE('',*,*,#5578,.F.);
#7160=ORIENTED_EDGE('',*,*,#5563,.T.);
#7161=ORIENTED_EDGE('',*,*,#5566,.T.);
#7162=ORIENTED_EDGE('',*,*,#5579,.T.);
#7163=ORIENTED_EDGE('',*,*,#5578,.T.);
#7164=ORIENTED_EDGE('',*,*,#5580,.F.);
#7165=ORIENTED_EDGE('',*,*,#5570,.F.);
#7166=ORIENTED_EDGE('',*,*,#5580,.T.);
#7167=ORIENTED_EDGE('',*,*,#5577,.T.);
#7168=ORIENTED_EDGE('',*,*,#5574,.T.);
#7169=ORIENTED_EDGE('',*,*,#5571,.T.);
#7170=ORIENTED_EDGE('',*,*,#5579,.F.);
#7171=ORIENTED_EDGE('',*,*,#5569,.F.);
#7172=ORIENTED_EDGE('',*,*,#5573,.F.);
#7173=ORIENTED_EDGE('',*,*,#5576,.F.);
#7174=ORIENTED_EDGE('',*,*,#5557,.T.);
#7175=ORIENTED_EDGE('',*,*,#5560,.T.);
#7176=ORIENTED_EDGE('',*,*,#5581,.F.);
#7177=ORIENTED_EDGE('',*,*,#5582,.T.);
#7178=ORIENTED_EDGE('',*,*,#5583,.F.);
#7179=ORIENTED_EDGE('',*,*,#5582,.F.);
#7180=ORIENTED_EDGE('',*,*,#5584,.F.);
#7181=ORIENTED_EDGE('',*,*,#5585,.T.);
#7182=ORIENTED_EDGE('',*,*,#5586,.F.);
#7183=ORIENTED_EDGE('',*,*,#5585,.F.);
#7184=ORIENTED_EDGE('',*,*,#5587,.F.);
#7185=ORIENTED_EDGE('',*,*,#5588,.T.);
#7186=ORIENTED_EDGE('',*,*,#5589,.T.);
#7187=ORIENTED_EDGE('',*,*,#5590,.F.);
#7188=ORIENTED_EDGE('',*,*,#5591,.F.);
#7189=ORIENTED_EDGE('',*,*,#5592,.F.);
#7190=ORIENTED_EDGE('',*,*,#5593,.T.);
#7191=ORIENTED_EDGE('',*,*,#5588,.F.);
#7192=ORIENTED_EDGE('',*,*,#5594,.F.);
#7193=ORIENTED_EDGE('',*,*,#5589,.F.);
#7194=ORIENTED_EDGE('',*,*,#5593,.F.);
#7195=ORIENTED_EDGE('',*,*,#5595,.F.);
#7196=ORIENTED_EDGE('',*,*,#5596,.T.);
#7197=ORIENTED_EDGE('',*,*,#5597,.T.);
#7198=ORIENTED_EDGE('',*,*,#5598,.F.);
#7199=ORIENTED_EDGE('',*,*,#5599,.F.);
#7200=ORIENTED_EDGE('',*,*,#5600,.F.);
#7201=ORIENTED_EDGE('',*,*,#5601,.T.);
#7202=ORIENTED_EDGE('',*,*,#5596,.F.);
#7203=ORIENTED_EDGE('',*,*,#5602,.F.);
#7204=ORIENTED_EDGE('',*,*,#5597,.F.);
#7205=ORIENTED_EDGE('',*,*,#5601,.F.);
#7206=ORIENTED_EDGE('',*,*,#5591,.T.);
#7207=ORIENTED_EDGE('',*,*,#5603,.T.);
#7208=ORIENTED_EDGE('',*,*,#5599,.T.);
#7209=ORIENTED_EDGE('',*,*,#5604,.T.);
#7210=ORIENTED_EDGE('',*,*,#5605,.F.);
#7211=ORIENTED_EDGE('',*,*,#5606,.T.);
#7212=ORIENTED_EDGE('',*,*,#5607,.T.);
#7213=ORIENTED_EDGE('',*,*,#5608,.T.);
#7214=ORIENTED_EDGE('',*,*,#5592,.T.);
#7215=ORIENTED_EDGE('',*,*,#5608,.F.);
#7216=ORIENTED_EDGE('',*,*,#5609,.T.);
#7217=ORIENTED_EDGE('',*,*,#5610,.F.);
#7218=ORIENTED_EDGE('',*,*,#5611,.F.);
#7219=ORIENTED_EDGE('',*,*,#5604,.F.);
#7220=ORIENTED_EDGE('',*,*,#5598,.T.);
#7221=ORIENTED_EDGE('',*,*,#5602,.T.);
#7222=ORIENTED_EDGE('',*,*,#5600,.T.);
#7223=ORIENTED_EDGE('',*,*,#5603,.F.);
#7224=ORIENTED_EDGE('',*,*,#5590,.T.);
#7225=ORIENTED_EDGE('',*,*,#5594,.T.);
#7226=ORIENTED_EDGE('',*,*,#5581,.T.);
#7227=ORIENTED_EDGE('',*,*,#5584,.T.);
#7228=ORIENTED_EDGE('',*,*,#5612,.T.);
#7229=ORIENTED_EDGE('',*,*,#5613,.T.);
#7230=ORIENTED_EDGE('',*,*,#5610,.T.);
#7231=ORIENTED_EDGE('',*,*,#5614,.T.);
#7232=ORIENTED_EDGE('',*,*,#5615,.F.);
#7233=ORIENTED_EDGE('',*,*,#5616,.T.);
#7234=ORIENTED_EDGE('',*,*,#5605,.T.);
#7235=ORIENTED_EDGE('',*,*,#5611,.T.);
#7236=ORIENTED_EDGE('',*,*,#5613,.F.);
#7237=ORIENTED_EDGE('',*,*,#5617,.F.);
#7238=ORIENTED_EDGE('',*,*,#5618,.F.);
#7239=ORIENTED_EDGE('',*,*,#5619,.T.);
#7240=ORIENTED_EDGE('',*,*,#5615,.T.);
#7241=ORIENTED_EDGE('',*,*,#5620,.F.);
#7242=ORIENTED_EDGE('',*,*,#5587,.T.);
#7243=ORIENTED_EDGE('',*,*,#5595,.T.);
#7244=ORIENTED_EDGE('',*,*,#5607,.F.);
#7245=ORIENTED_EDGE('',*,*,#5621,.T.);
#7246=ORIENTED_EDGE('',*,*,#5618,.T.);
#7247=ORIENTED_EDGE('',*,*,#5622,.T.);
#7248=ORIENTED_EDGE('',*,*,#5614,.F.);
#7249=ORIENTED_EDGE('',*,*,#5609,.F.);
#7250=ORIENTED_EDGE('',*,*,#5622,.F.);
#7251=ORIENTED_EDGE('',*,*,#5620,.T.);
#7252=ORIENTED_EDGE('',*,*,#5617,.T.);
#7253=ORIENTED_EDGE('',*,*,#5612,.F.);
#7254=ORIENTED_EDGE('',*,*,#5583,.T.);
#7255=ORIENTED_EDGE('',*,*,#5586,.T.);
#7256=ORIENTED_EDGE('',*,*,#5621,.F.);
#7257=ORIENTED_EDGE('',*,*,#5606,.F.);
#7258=ORIENTED_EDGE('',*,*,#5616,.F.);
#7259=ORIENTED_EDGE('',*,*,#5619,.F.);
#7260=ORIENTED_EDGE('',*,*,#5623,.F.);
#7261=ORIENTED_EDGE('',*,*,#5624,.T.);
#7262=ORIENTED_EDGE('',*,*,#5625,.T.);
#7263=ORIENTED_EDGE('',*,*,#5624,.F.);
#7264=ORIENTED_EDGE('',*,*,#5626,.F.);
#7265=ORIENTED_EDGE('',*,*,#5627,.T.);
#7266=ORIENTED_EDGE('',*,*,#5628,.T.);
#7267=ORIENTED_EDGE('',*,*,#5627,.F.);
#7268=ORIENTED_EDGE('',*,*,#5626,.T.);
#7269=ORIENTED_EDGE('',*,*,#5623,.T.);
#7270=ORIENTED_EDGE('',*,*,#5628,.F.);
#7271=ORIENTED_EDGE('',*,*,#5625,.F.);
#7272=ORIENTED_EDGE('',*,*,#5629,.T.);
#7273=ORIENTED_EDGE('',*,*,#5630,.T.);
#7274=ORIENTED_EDGE('',*,*,#5631,.F.);
#7275=ORIENTED_EDGE('',*,*,#5630,.F.);
#7276=ORIENTED_EDGE('',*,*,#5631,.T.);
#7277=ORIENTED_EDGE('',*,*,#5629,.F.);
#7278=ORIENTED_EDGE('',*,*,#5632,.F.);
#7279=ORIENTED_EDGE('',*,*,#5633,.T.);
#7280=ORIENTED_EDGE('',*,*,#5634,.T.);
#7281=ORIENTED_EDGE('',*,*,#5633,.F.);
#7282=ORIENTED_EDGE('',*,*,#5634,.F.);
#7283=ORIENTED_EDGE('',*,*,#5635,.F.);
#7284=ORIENTED_EDGE('',*,*,#5636,.T.);
#7285=ORIENTED_EDGE('',*,*,#5637,.T.);
#7286=ORIENTED_EDGE('',*,*,#5636,.F.);
#7287=ORIENTED_EDGE('',*,*,#5637,.F.);
#7288=ORIENTED_EDGE('',*,*,#5638,.F.);
#7289=ORIENTED_EDGE('',*,*,#5639,.T.);
#7290=ORIENTED_EDGE('',*,*,#5640,.T.);
#7291=ORIENTED_EDGE('',*,*,#5639,.F.);
#7292=ORIENTED_EDGE('',*,*,#5640,.F.);
#7293=ORIENTED_EDGE('',*,*,#5641,.F.);
#7294=ORIENTED_EDGE('',*,*,#5642,.T.);
#7295=ORIENTED_EDGE('',*,*,#5643,.T.);
#7296=ORIENTED_EDGE('',*,*,#5642,.F.);
#7297=ORIENTED_EDGE('',*,*,#5643,.F.);
#7298=ORIENTED_EDGE('',*,*,#5644,.F.);
#7299=ORIENTED_EDGE('',*,*,#5645,.T.);
#7300=ORIENTED_EDGE('',*,*,#5646,.F.);
#7301=ORIENTED_EDGE('',*,*,#5645,.F.);
#7302=ORIENTED_EDGE('',*,*,#5644,.T.);
#7303=ORIENTED_EDGE('',*,*,#5647,.F.);
#7304=ORIENTED_EDGE('',*,*,#5648,.T.);
#7305=ORIENTED_EDGE('',*,*,#5649,.F.);
#7306=ORIENTED_EDGE('',*,*,#5648,.F.);
#7307=ORIENTED_EDGE('',*,*,#5647,.T.);
#7308=ORIENTED_EDGE('',*,*,#5646,.T.);
#7309=ORIENTED_EDGE('',*,*,#5650,.T.);
#7310=ORIENTED_EDGE('',*,*,#5651,.T.);
#7311=ORIENTED_EDGE('',*,*,#5652,.F.);
#7312=ORIENTED_EDGE('',*,*,#5653,.F.);
#7313=ORIENTED_EDGE('',*,*,#5654,.T.);
#7314=ORIENTED_EDGE('',*,*,#5653,.T.);
#7315=ORIENTED_EDGE('',*,*,#5655,.F.);
#7316=ORIENTED_EDGE('',*,*,#5656,.F.);
#7317=ORIENTED_EDGE('',*,*,#5657,.T.);
#7318=ORIENTED_EDGE('',*,*,#5656,.T.);
#7319=ORIENTED_EDGE('',*,*,#5658,.F.);
#7320=ORIENTED_EDGE('',*,*,#5659,.F.);
#7321=ORIENTED_EDGE('',*,*,#5660,.T.);
#7322=ORIENTED_EDGE('',*,*,#5659,.T.);
#7323=ORIENTED_EDGE('',*,*,#5661,.F.);
#7324=ORIENTED_EDGE('',*,*,#5651,.F.);
#7325=ORIENTED_EDGE('',*,*,#5661,.T.);
#7326=ORIENTED_EDGE('',*,*,#5658,.T.);
#7327=ORIENTED_EDGE('',*,*,#5655,.T.);
#7328=ORIENTED_EDGE('',*,*,#5652,.T.);
#7329=ORIENTED_EDGE('',*,*,#5649,.T.);
#7330=ORIENTED_EDGE('',*,*,#5660,.F.);
#7331=ORIENTED_EDGE('',*,*,#5650,.F.);
#7332=ORIENTED_EDGE('',*,*,#5654,.F.);
#7333=ORIENTED_EDGE('',*,*,#5657,.F.);
#7334=ORIENTED_EDGE('',*,*,#5632,.T.);
#7335=ORIENTED_EDGE('',*,*,#5635,.T.);
#7336=ORIENTED_EDGE('',*,*,#5638,.T.);
#7337=ORIENTED_EDGE('',*,*,#5641,.T.);
#7338=ORIENTED_EDGE('',*,*,#5662,.F.);
#7339=ORIENTED_EDGE('',*,*,#5663,.T.);
#7340=ORIENTED_EDGE('',*,*,#5664,.F.);
#7341=ORIENTED_EDGE('',*,*,#5663,.F.);
#7342=ORIENTED_EDGE('',*,*,#5665,.F.);
#7343=ORIENTED_EDGE('',*,*,#5666,.T.);
#7344=ORIENTED_EDGE('',*,*,#5667,.F.);
#7345=ORIENTED_EDGE('',*,*,#5666,.F.);
#7346=ORIENTED_EDGE('',*,*,#5668,.F.);
#7347=ORIENTED_EDGE('',*,*,#5669,.T.);
#7348=ORIENTED_EDGE('',*,*,#5670,.F.);
#7349=ORIENTED_EDGE('',*,*,#5669,.F.);
#7350=ORIENTED_EDGE('',*,*,#5671,.F.);
#7351=ORIENTED_EDGE('',*,*,#5672,.T.);
#7352=ORIENTED_EDGE('',*,*,#5673,.F.);
#7353=ORIENTED_EDGE('',*,*,#5672,.F.);
#7354=ORIENTED_EDGE('',*,*,#5674,.F.);
#7355=ORIENTED_EDGE('',*,*,#5675,.T.);
#7356=ORIENTED_EDGE('',*,*,#5676,.F.);
#7357=ORIENTED_EDGE('',*,*,#5675,.F.);
#7358=ORIENTED_EDGE('',*,*,#5677,.F.);
#7359=ORIENTED_EDGE('',*,*,#5678,.T.);
#7360=ORIENTED_EDGE('',*,*,#5679,.F.);
#7361=ORIENTED_EDGE('',*,*,#5678,.F.);
#7362=ORIENTED_EDGE('',*,*,#5680,.F.);
#7363=ORIENTED_EDGE('',*,*,#5681,.T.);
#7364=ORIENTED_EDGE('',*,*,#5682,.F.);
#7365=ORIENTED_EDGE('',*,*,#5681,.F.);
#7366=ORIENTED_EDGE('',*,*,#5683,.F.);
#7367=ORIENTED_EDGE('',*,*,#5684,.T.);
#7368=ORIENTED_EDGE('',*,*,#5685,.F.);
#7369=ORIENTED_EDGE('',*,*,#5684,.F.);
#7370=ORIENTED_EDGE('',*,*,#5686,.T.);
#7371=ORIENTED_EDGE('',*,*,#5687,.T.);
#7372=ORIENTED_EDGE('',*,*,#5688,.F.);
#7373=ORIENTED_EDGE('',*,*,#5689,.F.);
#7374=ORIENTED_EDGE('',*,*,#5690,.T.);
#7375=ORIENTED_EDGE('',*,*,#5689,.T.);
#7376=ORIENTED_EDGE('',*,*,#5691,.F.);
#7377=ORIENTED_EDGE('',*,*,#5692,.F.);
#7378=ORIENTED_EDGE('',*,*,#5693,.T.);
#7379=ORIENTED_EDGE('',*,*,#5692,.T.);
#7380=ORIENTED_EDGE('',*,*,#5694,.F.);
#7381=ORIENTED_EDGE('',*,*,#5695,.F.);
#7382=ORIENTED_EDGE('',*,*,#5696,.T.);
#7383=ORIENTED_EDGE('',*,*,#5695,.T.);
#7384=ORIENTED_EDGE('',*,*,#5697,.F.);
#7385=ORIENTED_EDGE('',*,*,#5687,.F.);
#7386=ORIENTED_EDGE('',*,*,#5697,.T.);
#7387=ORIENTED_EDGE('',*,*,#5694,.T.);
#7388=ORIENTED_EDGE('',*,*,#5691,.T.);
#7389=ORIENTED_EDGE('',*,*,#5688,.T.);
#7390=ORIENTED_EDGE('',*,*,#5685,.T.);
#7391=ORIENTED_EDGE('',*,*,#5682,.T.);
#7392=ORIENTED_EDGE('',*,*,#5679,.T.);
#7393=ORIENTED_EDGE('',*,*,#5676,.T.);
#7394=ORIENTED_EDGE('',*,*,#5673,.T.);
#7395=ORIENTED_EDGE('',*,*,#5670,.T.);
#7396=ORIENTED_EDGE('',*,*,#5667,.T.);
#7397=ORIENTED_EDGE('',*,*,#5664,.T.);
#7398=ORIENTED_EDGE('',*,*,#5696,.F.);
#7399=ORIENTED_EDGE('',*,*,#5686,.F.);
#7400=ORIENTED_EDGE('',*,*,#5690,.F.);
#7401=ORIENTED_EDGE('',*,*,#5693,.F.);
#7402=ORIENTED_EDGE('',*,*,#5683,.T.);
#7403=ORIENTED_EDGE('',*,*,#5680,.T.);
#7404=ORIENTED_EDGE('',*,*,#5677,.T.);
#7405=ORIENTED_EDGE('',*,*,#5674,.T.);
#7406=ORIENTED_EDGE('',*,*,#5671,.T.);
#7407=ORIENTED_EDGE('',*,*,#5668,.T.);
#7408=ORIENTED_EDGE('',*,*,#5665,.T.);
#7409=ORIENTED_EDGE('',*,*,#5662,.T.);
#7410=ORIENTED_EDGE('',*,*,#5698,.F.);
#7411=ORIENTED_EDGE('',*,*,#5699,.T.);
#7412=ORIENTED_EDGE('',*,*,#5700,.T.);
#7413=ORIENTED_EDGE('',*,*,#5699,.F.);
#7414=ORIENTED_EDGE('',*,*,#5701,.F.);
#7415=ORIENTED_EDGE('',*,*,#5702,.T.);
#7416=ORIENTED_EDGE('',*,*,#5703,.T.);
#7417=ORIENTED_EDGE('',*,*,#5702,.F.);
#7418=ORIENTED_EDGE('',*,*,#5701,.T.);
#7419=ORIENTED_EDGE('',*,*,#5698,.T.);
#7420=ORIENTED_EDGE('',*,*,#5703,.F.);
#7421=ORIENTED_EDGE('',*,*,#5700,.F.);
#7422=ORIENTED_EDGE('',*,*,#5704,.F.);
#7423=ORIENTED_EDGE('',*,*,#5705,.T.);
#7424=ORIENTED_EDGE('',*,*,#5706,.T.);
#7425=ORIENTED_EDGE('',*,*,#5705,.F.);
#7426=ORIENTED_EDGE('',*,*,#5706,.F.);
#7427=ORIENTED_EDGE('',*,*,#5707,.F.);
#7428=ORIENTED_EDGE('',*,*,#5708,.T.);
#7429=ORIENTED_EDGE('',*,*,#5709,.T.);
#7430=ORIENTED_EDGE('',*,*,#5708,.F.);
#7431=ORIENTED_EDGE('',*,*,#5707,.T.);
#7432=ORIENTED_EDGE('',*,*,#5709,.F.);
#7433=ORIENTED_EDGE('',*,*,#5704,.T.);
#7434=ORIENTED_EDGE('',*,*,#5710,.F.);
#7435=ORIENTED_EDGE('',*,*,#5711,.T.);
#7436=ORIENTED_EDGE('',*,*,#5712,.T.);
#7437=ORIENTED_EDGE('',*,*,#5711,.F.);
#7438=ORIENTED_EDGE('',*,*,#5710,.T.);
#7439=ORIENTED_EDGE('',*,*,#5712,.F.);
#7440=ORIENTED_EDGE('',*,*,#5713,.F.);
#7441=ORIENTED_EDGE('',*,*,#5714,.T.);
#7442=ORIENTED_EDGE('',*,*,#5715,.F.);
#7443=ORIENTED_EDGE('',*,*,#5714,.F.);
#7444=ORIENTED_EDGE('',*,*,#5713,.T.);
#7445=ORIENTED_EDGE('',*,*,#5716,.F.);
#7446=ORIENTED_EDGE('',*,*,#5717,.T.);
#7447=ORIENTED_EDGE('',*,*,#5718,.T.);
#7448=ORIENTED_EDGE('',*,*,#5717,.F.);
#7449=ORIENTED_EDGE('',*,*,#5716,.T.);
#7450=ORIENTED_EDGE('',*,*,#5715,.T.);
#7451=ORIENTED_EDGE('',*,*,#5718,.F.);
#7452=ORIENTED_EDGE('',*,*,#5719,.F.);
#7453=ORIENTED_EDGE('',*,*,#5720,.T.);
#7454=ORIENTED_EDGE('',*,*,#5721,.T.);
#7455=ORIENTED_EDGE('',*,*,#5720,.F.);
#7456=ORIENTED_EDGE('',*,*,#5719,.T.);
#7457=ORIENTED_EDGE('',*,*,#5721,.F.);
#7458=ORIENTED_EDGE('',*,*,#5722,.F.);
#7459=ORIENTED_EDGE('',*,*,#5723,.T.);
#7460=ORIENTED_EDGE('',*,*,#5724,.T.);
#7461=ORIENTED_EDGE('',*,*,#5723,.F.);
#7462=ORIENTED_EDGE('',*,*,#5724,.F.);
#7463=ORIENTED_EDGE('',*,*,#5725,.F.);
#7464=ORIENTED_EDGE('',*,*,#5726,.T.);
#7465=ORIENTED_EDGE('',*,*,#5727,.T.);
#7466=ORIENTED_EDGE('',*,*,#5726,.F.);
#7467=ORIENTED_EDGE('',*,*,#5725,.T.);
#7468=ORIENTED_EDGE('',*,*,#5727,.F.);
#7469=ORIENTED_EDGE('',*,*,#5722,.T.);
#7470=ORIENTED_EDGE('',*,*,#5728,.F.);
#7471=ORIENTED_EDGE('',*,*,#5729,.T.);
#7472=ORIENTED_EDGE('',*,*,#5730,.T.);
#7473=ORIENTED_EDGE('',*,*,#5729,.F.);
#7474=ORIENTED_EDGE('',*,*,#5728,.T.);
#7475=ORIENTED_EDGE('',*,*,#5730,.F.);
#7476=ORIENTED_EDGE('',*,*,#5731,.F.);
#7477=ORIENTED_EDGE('',*,*,#5732,.T.);
#7478=ORIENTED_EDGE('',*,*,#5733,.F.);
#7479=ORIENTED_EDGE('',*,*,#5732,.F.);
#7480=ORIENTED_EDGE('',*,*,#5731,.T.);
#7481=ORIENTED_EDGE('',*,*,#5734,.F.);
#7482=ORIENTED_EDGE('',*,*,#5735,.T.);
#7483=ORIENTED_EDGE('',*,*,#5736,.T.);
#7484=ORIENTED_EDGE('',*,*,#5735,.F.);
#7485=ORIENTED_EDGE('',*,*,#5734,.T.);
#7486=ORIENTED_EDGE('',*,*,#5733,.T.);
#7487=ORIENTED_EDGE('',*,*,#5736,.F.);
#7488=ORIENTED_EDGE('',*,*,#5737,.F.);
#7489=ORIENTED_EDGE('',*,*,#5738,.T.);
#7490=ORIENTED_EDGE('',*,*,#5739,.T.);
#7491=ORIENTED_EDGE('',*,*,#5738,.F.);
#7492=ORIENTED_EDGE('',*,*,#5737,.T.);
#7493=ORIENTED_EDGE('',*,*,#5739,.F.);
#7494=ORIENTED_EDGE('',*,*,#5740,.T.);
#7495=ORIENTED_EDGE('',*,*,#5741,.T.);
#7496=ORIENTED_EDGE('',*,*,#5742,.T.);
#7497=ORIENTED_EDGE('',*,*,#5741,.F.);
#7498=ORIENTED_EDGE('',*,*,#5743,.F.);
#7499=ORIENTED_EDGE('',*,*,#5744,.T.);
#7500=ORIENTED_EDGE('',*,*,#5740,.F.);
#7501=ORIENTED_EDGE('',*,*,#5744,.F.);
#7502=ORIENTED_EDGE('',*,*,#5742,.F.);
#7503=ORIENTED_EDGE('',*,*,#5745,.T.);
#7504=ORIENTED_EDGE('',*,*,#5746,.T.);
#7505=ORIENTED_EDGE('',*,*,#5743,.T.);
#7506=ORIENTED_EDGE('',*,*,#5746,.F.);
#7507=ORIENTED_EDGE('',*,*,#5745,.F.);
#7508=ORIENTED_EDGE('',*,*,#5747,.F.);
#7509=ORIENTED_EDGE('',*,*,#5748,.F.);
#7510=ORIENTED_EDGE('',*,*,#5749,.F.);
#7511=ORIENTED_EDGE('',*,*,#5750,.F.);
#7512=ORIENTED_EDGE('',*,*,#5751,.F.);
#7513=ORIENTED_EDGE('',*,*,#5748,.T.);
#7514=ORIENTED_EDGE('',*,*,#5752,.F.);
#7515=ORIENTED_EDGE('',*,*,#5753,.T.);
#7516=ORIENTED_EDGE('',*,*,#5754,.F.);
#7517=ORIENTED_EDGE('',*,*,#5755,.F.);
#7518=ORIENTED_EDGE('',*,*,#5756,.F.);
#7519=ORIENTED_EDGE('',*,*,#5753,.F.);
#7520=ORIENTED_EDGE('',*,*,#5757,.T.);
#7521=ORIENTED_EDGE('',*,*,#5758,.F.);
#7522=ORIENTED_EDGE('',*,*,#5759,.T.);
#7523=ORIENTED_EDGE('',*,*,#5760,.F.);
#7524=ORIENTED_EDGE('',*,*,#5761,.T.);
#7525=ORIENTED_EDGE('',*,*,#5750,.T.);
#7526=ORIENTED_EDGE('',*,*,#5762,.T.);
#7527=ORIENTED_EDGE('',*,*,#5749,.T.);
#7528=ORIENTED_EDGE('',*,*,#5747,.T.);
#7529=ORIENTED_EDGE('',*,*,#5751,.T.);
#7530=ORIENTED_EDGE('',*,*,#5761,.F.);
#7531=ORIENTED_EDGE('',*,*,#5763,.F.);
#7532=ORIENTED_EDGE('',*,*,#5764,.T.);
#7533=ORIENTED_EDGE('',*,*,#5765,.F.);
#7534=ORIENTED_EDGE('',*,*,#5757,.F.);
#7535=ORIENTED_EDGE('',*,*,#5766,.T.);
#7536=ORIENTED_EDGE('',*,*,#5767,.T.);
#7537=ORIENTED_EDGE('',*,*,#5768,.F.);
#7538=ORIENTED_EDGE('',*,*,#5769,.F.);
#7539=ORIENTED_EDGE('',*,*,#5755,.T.);
#7540=ORIENTED_EDGE('',*,*,#5770,.F.);
#7541=ORIENTED_EDGE('',*,*,#5771,.F.);
#7542=ORIENTED_EDGE('',*,*,#5772,.T.);
#7543=ORIENTED_EDGE('',*,*,#5773,.F.);
#7544=ORIENTED_EDGE('',*,*,#5774,.T.);
#7545=ORIENTED_EDGE('',*,*,#5775,.F.);
#7546=ORIENTED_EDGE('',*,*,#5774,.F.);
#7547=ORIENTED_EDGE('',*,*,#5766,.F.);
#7548=ORIENTED_EDGE('',*,*,#5776,.T.);
#7549=ORIENTED_EDGE('',*,*,#5777,.F.);
#7550=ORIENTED_EDGE('',*,*,#5776,.F.);
#7551=ORIENTED_EDGE('',*,*,#5778,.F.);
#7552=ORIENTED_EDGE('',*,*,#5779,.T.);
#7553=ORIENTED_EDGE('',*,*,#5762,.F.);
#7554=ORIENTED_EDGE('',*,*,#5779,.F.);
#7555=ORIENTED_EDGE('',*,*,#5780,.F.);
#7556=ORIENTED_EDGE('',*,*,#5781,.T.);
#7557=ORIENTED_EDGE('',*,*,#5772,.F.);
#7558=ORIENTED_EDGE('',*,*,#5781,.F.);
#7559=ORIENTED_EDGE('',*,*,#5782,.F.);
#7560=ORIENTED_EDGE('',*,*,#5783,.T.);
#7561=ORIENTED_EDGE('',*,*,#5784,.F.);
#7562=ORIENTED_EDGE('',*,*,#5783,.F.);
#7563=ORIENTED_EDGE('',*,*,#5760,.T.);
#7564=ORIENTED_EDGE('',*,*,#5785,.T.);
#7565=ORIENTED_EDGE('',*,*,#5786,.T.);
#7566=ORIENTED_EDGE('',*,*,#5787,.T.);
#7567=ORIENTED_EDGE('',*,*,#5771,.T.);
#7568=ORIENTED_EDGE('',*,*,#5788,.T.);
#7569=ORIENTED_EDGE('',*,*,#5789,.T.);
#7570=ORIENTED_EDGE('',*,*,#5790,.T.);
#7571=ORIENTED_EDGE('',*,*,#5791,.T.);
#7572=ORIENTED_EDGE('',*,*,#5792,.T.);
#7573=ORIENTED_EDGE('',*,*,#5793,.T.);
#7574=ORIENTED_EDGE('',*,*,#5763,.T.);
#7575=ORIENTED_EDGE('',*,*,#5782,.T.);
#7576=ORIENTED_EDGE('',*,*,#5759,.F.);
#7577=ORIENTED_EDGE('',*,*,#5794,.F.);
#7578=ORIENTED_EDGE('',*,*,#5795,.F.);
#7579=ORIENTED_EDGE('',*,*,#5785,.F.);
#7580=ORIENTED_EDGE('',*,*,#5795,.T.);
#7581=ORIENTED_EDGE('',*,*,#5796,.F.);
#7582=ORIENTED_EDGE('',*,*,#5797,.F.);
#7583=ORIENTED_EDGE('',*,*,#5786,.F.);
#7584=ORIENTED_EDGE('',*,*,#5778,.T.);
#7585=ORIENTED_EDGE('',*,*,#5780,.T.);
#7586=ORIENTED_EDGE('',*,*,#5797,.T.);
#7587=ORIENTED_EDGE('',*,*,#5798,.F.);
#7588=ORIENTED_EDGE('',*,*,#5767,.F.);
#7589=ORIENTED_EDGE('',*,*,#5787,.F.);
#7590=ORIENTED_EDGE('',*,*,#5752,.T.);
#7591=ORIENTED_EDGE('',*,*,#5769,.T.);
#7592=ORIENTED_EDGE('',*,*,#5799,.F.);
#7593=ORIENTED_EDGE('',*,*,#5800,.F.);
#7594=ORIENTED_EDGE('',*,*,#5788,.F.);
#7595=ORIENTED_EDGE('',*,*,#5770,.T.);
#7596=ORIENTED_EDGE('',*,*,#5754,.T.);
#7597=ORIENTED_EDGE('',*,*,#5756,.T.);
#7598=ORIENTED_EDGE('',*,*,#5775,.T.);
#7599=ORIENTED_EDGE('',*,*,#5800,.T.);
#7600=ORIENTED_EDGE('',*,*,#5801,.F.);
#7601=ORIENTED_EDGE('',*,*,#5802,.F.);
#7602=ORIENTED_EDGE('',*,*,#5789,.F.);
#7603=ORIENTED_EDGE('',*,*,#5802,.T.);
#7604=ORIENTED_EDGE('',*,*,#5803,.F.);
#7605=ORIENTED_EDGE('',*,*,#5804,.F.);
#7606=ORIENTED_EDGE('',*,*,#5790,.F.);
#7607=ORIENTED_EDGE('',*,*,#5773,.T.);
#7608=ORIENTED_EDGE('',*,*,#5804,.T.);
#7609=ORIENTED_EDGE('',*,*,#5805,.F.);
#7610=ORIENTED_EDGE('',*,*,#5806,.F.);
#7611=ORIENTED_EDGE('',*,*,#5791,.F.);
#7612=ORIENTED_EDGE('',*,*,#5806,.T.);
#7613=ORIENTED_EDGE('',*,*,#5807,.F.);
#7614=ORIENTED_EDGE('',*,*,#5808,.F.);
#7615=ORIENTED_EDGE('',*,*,#5792,.F.);
#7616=ORIENTED_EDGE('',*,*,#5777,.T.);
#7617=ORIENTED_EDGE('',*,*,#5808,.T.);
#7618=ORIENTED_EDGE('',*,*,#5809,.F.);
#7619=ORIENTED_EDGE('',*,*,#5764,.F.);
#7620=ORIENTED_EDGE('',*,*,#5793,.F.);
#7621=ORIENTED_EDGE('',*,*,#5758,.T.);
#7622=ORIENTED_EDGE('',*,*,#5765,.T.);
#7623=ORIENTED_EDGE('',*,*,#5809,.T.);
#7624=ORIENTED_EDGE('',*,*,#5807,.T.);
#7625=ORIENTED_EDGE('',*,*,#5805,.T.);
#7626=ORIENTED_EDGE('',*,*,#5803,.T.);
#7627=ORIENTED_EDGE('',*,*,#5801,.T.);
#7628=ORIENTED_EDGE('',*,*,#5799,.T.);
#7629=ORIENTED_EDGE('',*,*,#5768,.T.);
#7630=ORIENTED_EDGE('',*,*,#5798,.T.);
#7631=ORIENTED_EDGE('',*,*,#5796,.T.);
#7632=ORIENTED_EDGE('',*,*,#5794,.T.);
#7633=ORIENTED_EDGE('',*,*,#5784,.T.);
#7634=ORIENTED_EDGE('',*,*,#5810,.T.);
#7635=ORIENTED_EDGE('',*,*,#5811,.T.);
#7636=ORIENTED_EDGE('',*,*,#5812,.T.);
#7637=ORIENTED_EDGE('',*,*,#5813,.F.);
#7638=ORIENTED_EDGE('',*,*,#5814,.T.);
#7639=ORIENTED_EDGE('',*,*,#5815,.T.);
#7640=ORIENTED_EDGE('',*,*,#5816,.T.);
#7641=ORIENTED_EDGE('',*,*,#5811,.F.);
#7642=ORIENTED_EDGE('',*,*,#5817,.T.);
#7643=ORIENTED_EDGE('',*,*,#5818,.T.);
#7644=ORIENTED_EDGE('',*,*,#5819,.T.);
#7645=ORIENTED_EDGE('',*,*,#5815,.F.);
#7646=ORIENTED_EDGE('',*,*,#5820,.T.);
#7647=ORIENTED_EDGE('',*,*,#5821,.T.);
#7648=ORIENTED_EDGE('',*,*,#5822,.T.);
#7649=ORIENTED_EDGE('',*,*,#5818,.F.);
#7650=ORIENTED_EDGE('',*,*,#5823,.T.);
#7651=ORIENTED_EDGE('',*,*,#5824,.T.);
#7652=ORIENTED_EDGE('',*,*,#5825,.T.);
#7653=ORIENTED_EDGE('',*,*,#5821,.F.);
#7654=ORIENTED_EDGE('',*,*,#5826,.T.);
#7655=ORIENTED_EDGE('',*,*,#5813,.T.);
#7656=ORIENTED_EDGE('',*,*,#5827,.T.);
#7657=ORIENTED_EDGE('',*,*,#5824,.F.);
#7658=ORIENTED_EDGE('',*,*,#5826,.F.);
#7659=ORIENTED_EDGE('',*,*,#5823,.F.);
#7660=ORIENTED_EDGE('',*,*,#5820,.F.);
#7661=ORIENTED_EDGE('',*,*,#5817,.F.);
#7662=ORIENTED_EDGE('',*,*,#5814,.F.);
#7663=ORIENTED_EDGE('',*,*,#5810,.F.);
#7664=ORIENTED_EDGE('',*,*,#5827,.F.);
#7665=ORIENTED_EDGE('',*,*,#5812,.F.);
#7666=ORIENTED_EDGE('',*,*,#5816,.F.);
#7667=ORIENTED_EDGE('',*,*,#5819,.F.);
#7668=ORIENTED_EDGE('',*,*,#5822,.F.);
#7669=ORIENTED_EDGE('',*,*,#5825,.F.);
#7670=ORIENTED_EDGE('',*,*,#5828,.F.);
#7671=ORIENTED_EDGE('',*,*,#5829,.F.);
#7672=ORIENTED_EDGE('',*,*,#5830,.F.);
#7673=ORIENTED_EDGE('',*,*,#5831,.T.);
#7674=ORIENTED_EDGE('',*,*,#5829,.T.);
#7675=ORIENTED_EDGE('',*,*,#5831,.F.);
#7676=ORIENTED_EDGE('',*,*,#5832,.F.);
#7677=ORIENTED_EDGE('',*,*,#5833,.T.);
#7678=ORIENTED_EDGE('',*,*,#5830,.T.);
#7679=ORIENTED_EDGE('',*,*,#5833,.F.);
#7680=ORIENTED_EDGE('',*,*,#5834,.F.);
#7681=ORIENTED_EDGE('',*,*,#5835,.T.);
#7682=ORIENTED_EDGE('',*,*,#5832,.T.);
#7683=ORIENTED_EDGE('',*,*,#5835,.F.);
#7684=ORIENTED_EDGE('',*,*,#5834,.T.);
#7685=ORIENTED_EDGE('',*,*,#5836,.F.);
#7686=ORIENTED_EDGE('',*,*,#5837,.F.);
#7687=ORIENTED_EDGE('',*,*,#5838,.T.);
#7688=ORIENTED_EDGE('',*,*,#5836,.T.);
#7689=ORIENTED_EDGE('',*,*,#5838,.F.);
#7690=ORIENTED_EDGE('',*,*,#5828,.T.);
#7691=ORIENTED_EDGE('',*,*,#5839,.T.);
#7692=ORIENTED_EDGE('',*,*,#5837,.T.);
#7693=ORIENTED_EDGE('',*,*,#5839,.F.);
#7694=ORIENTED_EDGE('',*,*,#5840,.F.);
#7695=ORIENTED_EDGE('',*,*,#5841,.F.);
#7696=ORIENTED_EDGE('',*,*,#5842,.T.);
#7697=ORIENTED_EDGE('',*,*,#5840,.T.);
#7698=ORIENTED_EDGE('',*,*,#5842,.F.);
#7699=ORIENTED_EDGE('',*,*,#5843,.F.);
#7700=ORIENTED_EDGE('',*,*,#5844,.T.);
#7701=ORIENTED_EDGE('',*,*,#5841,.T.);
#7702=ORIENTED_EDGE('',*,*,#5844,.F.);
#7703=ORIENTED_EDGE('',*,*,#5845,.F.);
#7704=ORIENTED_EDGE('',*,*,#5846,.T.);
#7705=ORIENTED_EDGE('',*,*,#5843,.T.);
#7706=ORIENTED_EDGE('',*,*,#5846,.F.);
#7707=ORIENTED_EDGE('',*,*,#5845,.T.);
#7708=ORIENTED_EDGE('',*,*,#5847,.F.);
#7709=ORIENTED_EDGE('',*,*,#5848,.F.);
#7710=ORIENTED_EDGE('',*,*,#5849,.T.);
#7711=ORIENTED_EDGE('',*,*,#5847,.T.);
#7712=ORIENTED_EDGE('',*,*,#5849,.F.);
#7713=ORIENTED_EDGE('',*,*,#5850,.F.);
#7714=ORIENTED_EDGE('',*,*,#5851,.T.);
#7715=ORIENTED_EDGE('',*,*,#5848,.T.);
#7716=ORIENTED_EDGE('',*,*,#5851,.F.);
#7717=ORIENTED_EDGE('',*,*,#5852,.F.);
#7718=ORIENTED_EDGE('',*,*,#5853,.T.);
#7719=ORIENTED_EDGE('',*,*,#5850,.T.);
#7720=ORIENTED_EDGE('',*,*,#5853,.F.);
#7721=ORIENTED_EDGE('',*,*,#5852,.T.);
#7722=ORIENTED_EDGE('',*,*,#5854,.T.);
#7723=ORIENTED_EDGE('',*,*,#5855,.T.);
#7724=ORIENTED_EDGE('',*,*,#5856,.T.);
#7725=ORIENTED_EDGE('',*,*,#5857,.F.);
#7726=ORIENTED_EDGE('',*,*,#5858,.T.);
#7727=ORIENTED_EDGE('',*,*,#5859,.T.);
#7728=ORIENTED_EDGE('',*,*,#5860,.T.);
#7729=ORIENTED_EDGE('',*,*,#5855,.F.);
#7730=ORIENTED_EDGE('',*,*,#5861,.T.);
#7731=ORIENTED_EDGE('',*,*,#5862,.T.);
#7732=ORIENTED_EDGE('',*,*,#5863,.T.);
#7733=ORIENTED_EDGE('',*,*,#5859,.F.);
#7734=ORIENTED_EDGE('',*,*,#5864,.T.);
#7735=ORIENTED_EDGE('',*,*,#5865,.T.);
#7736=ORIENTED_EDGE('',*,*,#5866,.T.);
#7737=ORIENTED_EDGE('',*,*,#5862,.F.);
#7738=ORIENTED_EDGE('',*,*,#5867,.T.);
#7739=ORIENTED_EDGE('',*,*,#5868,.T.);
#7740=ORIENTED_EDGE('',*,*,#5869,.T.);
#7741=ORIENTED_EDGE('',*,*,#5865,.F.);
#7742=ORIENTED_EDGE('',*,*,#5870,.T.);
#7743=ORIENTED_EDGE('',*,*,#5857,.T.);
#7744=ORIENTED_EDGE('',*,*,#5871,.T.);
#7745=ORIENTED_EDGE('',*,*,#5868,.F.);
#7746=ORIENTED_EDGE('',*,*,#5870,.F.);
#7747=ORIENTED_EDGE('',*,*,#5867,.F.);
#7748=ORIENTED_EDGE('',*,*,#5864,.F.);
#7749=ORIENTED_EDGE('',*,*,#5861,.F.);
#7750=ORIENTED_EDGE('',*,*,#5858,.F.);
#7751=ORIENTED_EDGE('',*,*,#5854,.F.);
#7752=ORIENTED_EDGE('',*,*,#5871,.F.);
#7753=ORIENTED_EDGE('',*,*,#5856,.F.);
#7754=ORIENTED_EDGE('',*,*,#5860,.F.);
#7755=ORIENTED_EDGE('',*,*,#5863,.F.);
#7756=ORIENTED_EDGE('',*,*,#5866,.F.);
#7757=ORIENTED_EDGE('',*,*,#5869,.F.);
#7758=ORIENTED_EDGE('',*,*,#5872,.F.);
#7759=ORIENTED_EDGE('',*,*,#5873,.T.);
#7760=ORIENTED_EDGE('',*,*,#5874,.F.);
#7761=ORIENTED_EDGE('',*,*,#5873,.F.);
#7762=ORIENTED_EDGE('',*,*,#5875,.F.);
#7763=ORIENTED_EDGE('',*,*,#5876,.T.);
#7764=ORIENTED_EDGE('',*,*,#5877,.F.);
#7765=ORIENTED_EDGE('',*,*,#5876,.F.);
#7766=ORIENTED_EDGE('',*,*,#5878,.F.);
#7767=ORIENTED_EDGE('',*,*,#5879,.T.);
#7768=ORIENTED_EDGE('',*,*,#5880,.F.);
#7769=ORIENTED_EDGE('',*,*,#5879,.F.);
#7770=ORIENTED_EDGE('',*,*,#5881,.F.);
#7771=ORIENTED_EDGE('',*,*,#5882,.T.);
#7772=ORIENTED_EDGE('',*,*,#5883,.F.);
#7773=ORIENTED_EDGE('',*,*,#5882,.F.);
#7774=ORIENTED_EDGE('',*,*,#5884,.F.);
#7775=ORIENTED_EDGE('',*,*,#5885,.T.);
#7776=ORIENTED_EDGE('',*,*,#5886,.F.);
#7777=ORIENTED_EDGE('',*,*,#5885,.F.);
#7778=ORIENTED_EDGE('',*,*,#5887,.F.);
#7779=ORIENTED_EDGE('',*,*,#5888,.T.);
#7780=ORIENTED_EDGE('',*,*,#5889,.F.);
#7781=ORIENTED_EDGE('',*,*,#5888,.F.);
#7782=ORIENTED_EDGE('',*,*,#5890,.F.);
#7783=ORIENTED_EDGE('',*,*,#5891,.T.);
#7784=ORIENTED_EDGE('',*,*,#5892,.F.);
#7785=ORIENTED_EDGE('',*,*,#5891,.F.);
#7786=ORIENTED_EDGE('',*,*,#5893,.F.);
#7787=ORIENTED_EDGE('',*,*,#5894,.T.);
#7788=ORIENTED_EDGE('',*,*,#5895,.F.);
#7789=ORIENTED_EDGE('',*,*,#5894,.F.);
#7790=ORIENTED_EDGE('',*,*,#5896,.F.);
#7791=ORIENTED_EDGE('',*,*,#5897,.T.);
#7792=ORIENTED_EDGE('',*,*,#5898,.F.);
#7793=ORIENTED_EDGE('',*,*,#5897,.F.);
#7794=ORIENTED_EDGE('',*,*,#5899,.F.);
#7795=ORIENTED_EDGE('',*,*,#5900,.T.);
#7796=ORIENTED_EDGE('',*,*,#5901,.F.);
#7797=ORIENTED_EDGE('',*,*,#5900,.F.);
#7798=ORIENTED_EDGE('',*,*,#5902,.F.);
#7799=ORIENTED_EDGE('',*,*,#5903,.T.);
#7800=ORIENTED_EDGE('',*,*,#5904,.F.);
#7801=ORIENTED_EDGE('',*,*,#5903,.F.);
#7802=ORIENTED_EDGE('',*,*,#5905,.F.);
#7803=ORIENTED_EDGE('',*,*,#5906,.T.);
#7804=ORIENTED_EDGE('',*,*,#5907,.F.);
#7805=ORIENTED_EDGE('',*,*,#5906,.F.);
#7806=ORIENTED_EDGE('',*,*,#5908,.F.);
#7807=ORIENTED_EDGE('',*,*,#5909,.T.);
#7808=ORIENTED_EDGE('',*,*,#5910,.F.);
#7809=ORIENTED_EDGE('',*,*,#5909,.F.);
#7810=ORIENTED_EDGE('',*,*,#5911,.F.);
#7811=ORIENTED_EDGE('',*,*,#5912,.T.);
#7812=ORIENTED_EDGE('',*,*,#5913,.F.);
#7813=ORIENTED_EDGE('',*,*,#5912,.F.);
#7814=ORIENTED_EDGE('',*,*,#5914,.F.);
#7815=ORIENTED_EDGE('',*,*,#5915,.T.);
#7816=ORIENTED_EDGE('',*,*,#5916,.F.);
#7817=ORIENTED_EDGE('',*,*,#5915,.F.);
#7818=ORIENTED_EDGE('',*,*,#5917,.F.);
#7819=ORIENTED_EDGE('',*,*,#5918,.T.);
#7820=ORIENTED_EDGE('',*,*,#5919,.F.);
#7821=ORIENTED_EDGE('',*,*,#5918,.F.);
#7822=ORIENTED_EDGE('',*,*,#5920,.F.);
#7823=ORIENTED_EDGE('',*,*,#5921,.T.);
#7824=ORIENTED_EDGE('',*,*,#5922,.F.);
#7825=ORIENTED_EDGE('',*,*,#5921,.F.);
#7826=ORIENTED_EDGE('',*,*,#5923,.F.);
#7827=ORIENTED_EDGE('',*,*,#5924,.T.);
#7828=ORIENTED_EDGE('',*,*,#5925,.F.);
#7829=ORIENTED_EDGE('',*,*,#5924,.F.);
#7830=ORIENTED_EDGE('',*,*,#5926,.F.);
#7831=ORIENTED_EDGE('',*,*,#5927,.T.);
#7832=ORIENTED_EDGE('',*,*,#5928,.F.);
#7833=ORIENTED_EDGE('',*,*,#5927,.F.);
#7834=ORIENTED_EDGE('',*,*,#5929,.F.);
#7835=ORIENTED_EDGE('',*,*,#5930,.T.);
#7836=ORIENTED_EDGE('',*,*,#5931,.F.);
#7837=ORIENTED_EDGE('',*,*,#5930,.F.);
#7838=ORIENTED_EDGE('',*,*,#5932,.F.);
#7839=ORIENTED_EDGE('',*,*,#5933,.T.);
#7840=ORIENTED_EDGE('',*,*,#5934,.F.);
#7841=ORIENTED_EDGE('',*,*,#5933,.F.);
#7842=ORIENTED_EDGE('',*,*,#5935,.F.);
#7843=ORIENTED_EDGE('',*,*,#5936,.T.);
#7844=ORIENTED_EDGE('',*,*,#5937,.F.);
#7845=ORIENTED_EDGE('',*,*,#5936,.F.);
#7846=ORIENTED_EDGE('',*,*,#5938,.F.);
#7847=ORIENTED_EDGE('',*,*,#5939,.T.);
#7848=ORIENTED_EDGE('',*,*,#5940,.F.);
#7849=ORIENTED_EDGE('',*,*,#5939,.F.);
#7850=ORIENTED_EDGE('',*,*,#5941,.F.);
#7851=ORIENTED_EDGE('',*,*,#5942,.T.);
#7852=ORIENTED_EDGE('',*,*,#5943,.F.);
#7853=ORIENTED_EDGE('',*,*,#5942,.F.);
#7854=ORIENTED_EDGE('',*,*,#5944,.T.);
#7855=ORIENTED_EDGE('',*,*,#5945,.T.);
#7856=ORIENTED_EDGE('',*,*,#5946,.F.);
#7857=ORIENTED_EDGE('',*,*,#5947,.F.);
#7858=ORIENTED_EDGE('',*,*,#5948,.T.);
#7859=ORIENTED_EDGE('',*,*,#5947,.T.);
#7860=ORIENTED_EDGE('',*,*,#5949,.F.);
#7861=ORIENTED_EDGE('',*,*,#5950,.F.);
#7862=ORIENTED_EDGE('',*,*,#5951,.T.);
#7863=ORIENTED_EDGE('',*,*,#5950,.T.);
#7864=ORIENTED_EDGE('',*,*,#5952,.F.);
#7865=ORIENTED_EDGE('',*,*,#5953,.F.);
#7866=ORIENTED_EDGE('',*,*,#5954,.T.);
#7867=ORIENTED_EDGE('',*,*,#5953,.T.);
#7868=ORIENTED_EDGE('',*,*,#5955,.F.);
#7869=ORIENTED_EDGE('',*,*,#5945,.F.);
#7870=ORIENTED_EDGE('',*,*,#5955,.T.);
#7871=ORIENTED_EDGE('',*,*,#5952,.T.);
#7872=ORIENTED_EDGE('',*,*,#5949,.T.);
#7873=ORIENTED_EDGE('',*,*,#5946,.T.);
#7874=ORIENTED_EDGE('',*,*,#5886,.T.);
#7875=ORIENTED_EDGE('',*,*,#5889,.T.);
#7876=ORIENTED_EDGE('',*,*,#5892,.T.);
#7877=ORIENTED_EDGE('',*,*,#5895,.T.);
#7878=ORIENTED_EDGE('',*,*,#5910,.T.);
#7879=ORIENTED_EDGE('',*,*,#5913,.T.);
#7880=ORIENTED_EDGE('',*,*,#5916,.T.);
#7881=ORIENTED_EDGE('',*,*,#5919,.T.);
#7882=ORIENTED_EDGE('',*,*,#5943,.T.);
#7883=ORIENTED_EDGE('',*,*,#5940,.T.);
#7884=ORIENTED_EDGE('',*,*,#5937,.T.);
#7885=ORIENTED_EDGE('',*,*,#5934,.T.);
#7886=ORIENTED_EDGE('',*,*,#5931,.T.);
#7887=ORIENTED_EDGE('',*,*,#5928,.T.);
#7888=ORIENTED_EDGE('',*,*,#5925,.T.);
#7889=ORIENTED_EDGE('',*,*,#5922,.T.);
#7890=ORIENTED_EDGE('',*,*,#5907,.T.);
#7891=ORIENTED_EDGE('',*,*,#5904,.T.);
#7892=ORIENTED_EDGE('',*,*,#5901,.T.);
#7893=ORIENTED_EDGE('',*,*,#5898,.T.);
#7894=ORIENTED_EDGE('',*,*,#5883,.T.);
#7895=ORIENTED_EDGE('',*,*,#5880,.T.);
#7896=ORIENTED_EDGE('',*,*,#5877,.T.);
#7897=ORIENTED_EDGE('',*,*,#5874,.T.);
#7898=ORIENTED_EDGE('',*,*,#5954,.F.);
#7899=ORIENTED_EDGE('',*,*,#5944,.F.);
#7900=ORIENTED_EDGE('',*,*,#5948,.F.);
#7901=ORIENTED_EDGE('',*,*,#5951,.F.);
#7902=ORIENTED_EDGE('',*,*,#5884,.T.);
#7903=ORIENTED_EDGE('',*,*,#5887,.T.);
#7904=ORIENTED_EDGE('',*,*,#5890,.T.);
#7905=ORIENTED_EDGE('',*,*,#5893,.T.);
#7906=ORIENTED_EDGE('',*,*,#5908,.T.);
#7907=ORIENTED_EDGE('',*,*,#5911,.T.);
#7908=ORIENTED_EDGE('',*,*,#5914,.T.);
#7909=ORIENTED_EDGE('',*,*,#5917,.T.);
#7910=ORIENTED_EDGE('',*,*,#5941,.T.);
#7911=ORIENTED_EDGE('',*,*,#5938,.T.);
#7912=ORIENTED_EDGE('',*,*,#5935,.T.);
#7913=ORIENTED_EDGE('',*,*,#5932,.T.);
#7914=ORIENTED_EDGE('',*,*,#5929,.T.);
#7915=ORIENTED_EDGE('',*,*,#5926,.T.);
#7916=ORIENTED_EDGE('',*,*,#5923,.T.);
#7917=ORIENTED_EDGE('',*,*,#5920,.T.);
#7918=ORIENTED_EDGE('',*,*,#5905,.T.);
#7919=ORIENTED_EDGE('',*,*,#5902,.T.);
#7920=ORIENTED_EDGE('',*,*,#5899,.T.);
#7921=ORIENTED_EDGE('',*,*,#5896,.T.);
#7922=ORIENTED_EDGE('',*,*,#5881,.T.);
#7923=ORIENTED_EDGE('',*,*,#5878,.T.);
#7924=ORIENTED_EDGE('',*,*,#5875,.T.);
#7925=ORIENTED_EDGE('',*,*,#5872,.T.);
#7926=ORIENTED_EDGE('',*,*,#5956,.F.);
#7927=ORIENTED_EDGE('',*,*,#5957,.T.);
#7928=ORIENTED_EDGE('',*,*,#5958,.F.);
#7929=ORIENTED_EDGE('',*,*,#5959,.F.);
#7930=ORIENTED_EDGE('',*,*,#5960,.T.);
#7931=ORIENTED_EDGE('',*,*,#5961,.F.);
#7932=ORIENTED_EDGE('',*,*,#5960,.F.);
#7933=ORIENTED_EDGE('',*,*,#5962,.F.);
#7934=ORIENTED_EDGE('',*,*,#5963,.F.);
#7935=ORIENTED_EDGE('',*,*,#5957,.F.);
#7936=ORIENTED_EDGE('',*,*,#5964,.F.);
#7937=ORIENTED_EDGE('',*,*,#5965,.T.);
#7938=ORIENTED_EDGE('',*,*,#5966,.F.);
#7939=ORIENTED_EDGE('',*,*,#5967,.F.);
#7940=ORIENTED_EDGE('',*,*,#5968,.T.);
#7941=ORIENTED_EDGE('',*,*,#5969,.F.);
#7942=ORIENTED_EDGE('',*,*,#5968,.F.);
#7943=ORIENTED_EDGE('',*,*,#5970,.F.);
#7944=ORIENTED_EDGE('',*,*,#5971,.F.);
#7945=ORIENTED_EDGE('',*,*,#5965,.F.);
#7946=ORIENTED_EDGE('',*,*,#5972,.F.);
#7947=ORIENTED_EDGE('',*,*,#5973,.T.);
#7948=ORIENTED_EDGE('',*,*,#5974,.T.);
#7949=ORIENTED_EDGE('',*,*,#5975,.F.);
#7950=ORIENTED_EDGE('',*,*,#5976,.F.);
#7951=ORIENTED_EDGE('',*,*,#5977,.F.);
#7952=ORIENTED_EDGE('',*,*,#5974,.F.);
#7953=ORIENTED_EDGE('',*,*,#5978,.T.);
#7954=ORIENTED_EDGE('',*,*,#5979,.F.);
#7955=ORIENTED_EDGE('',*,*,#5978,.F.);
#7956=ORIENTED_EDGE('',*,*,#5973,.F.);
#7957=ORIENTED_EDGE('',*,*,#5980,.F.);
#7958=ORIENTED_EDGE('',*,*,#5981,.T.);
#7959=ORIENTED_EDGE('',*,*,#5982,.T.);
#7960=ORIENTED_EDGE('',*,*,#5983,.F.);
#7961=ORIENTED_EDGE('',*,*,#5984,.F.);
#7962=ORIENTED_EDGE('',*,*,#5985,.F.);
#7963=ORIENTED_EDGE('',*,*,#5982,.F.);
#7964=ORIENTED_EDGE('',*,*,#5986,.T.);
#7965=ORIENTED_EDGE('',*,*,#5987,.F.);
#7966=ORIENTED_EDGE('',*,*,#5986,.F.);
#7967=ORIENTED_EDGE('',*,*,#5981,.F.);
#7968=ORIENTED_EDGE('',*,*,#5958,.T.);
#7969=ORIENTED_EDGE('',*,*,#5956,.T.);
#7970=ORIENTED_EDGE('',*,*,#5963,.T.);
#7971=ORIENTED_EDGE('',*,*,#5988,.T.);
#7972=ORIENTED_EDGE('',*,*,#5989,.T.);
#7973=ORIENTED_EDGE('',*,*,#5990,.T.);
#7974=ORIENTED_EDGE('',*,*,#5989,.F.);
#7975=ORIENTED_EDGE('',*,*,#5991,.T.);
#7976=ORIENTED_EDGE('',*,*,#5966,.T.);
#7977=ORIENTED_EDGE('',*,*,#5964,.T.);
#7978=ORIENTED_EDGE('',*,*,#5971,.T.);
#7979=ORIENTED_EDGE('',*,*,#5992,.T.);
#7980=ORIENTED_EDGE('',*,*,#5975,.T.);
#7981=ORIENTED_EDGE('',*,*,#5972,.T.);
#7982=ORIENTED_EDGE('',*,*,#5977,.T.);
#7983=ORIENTED_EDGE('',*,*,#5993,.T.);
#7984=ORIENTED_EDGE('',*,*,#5983,.T.);
#7985=ORIENTED_EDGE('',*,*,#5980,.T.);
#7986=ORIENTED_EDGE('',*,*,#5985,.T.);
#7987=ORIENTED_EDGE('',*,*,#5994,.T.);
#7988=ORIENTED_EDGE('',*,*,#5995,.F.);
#7989=ORIENTED_EDGE('',*,*,#5996,.T.);
#7990=ORIENTED_EDGE('',*,*,#5997,.F.);
#7991=ORIENTED_EDGE('',*,*,#5996,.F.);
#7992=ORIENTED_EDGE('',*,*,#5995,.T.);
#7993=ORIENTED_EDGE('',*,*,#5998,.F.);
#7994=ORIENTED_EDGE('',*,*,#5999,.F.);
#7995=ORIENTED_EDGE('',*,*,#5962,.T.);
#7996=ORIENTED_EDGE('',*,*,#5959,.T.);
#7997=ORIENTED_EDGE('',*,*,#5994,.F.);
#7998=ORIENTED_EDGE('',*,*,#5984,.T.);
#7999=ORIENTED_EDGE('',*,*,#5993,.F.);
#8000=ORIENTED_EDGE('',*,*,#5976,.T.);
#8001=ORIENTED_EDGE('',*,*,#5992,.F.);
#8002=ORIENTED_EDGE('',*,*,#5970,.T.);
#8003=ORIENTED_EDGE('',*,*,#5967,.T.);
#8004=ORIENTED_EDGE('',*,*,#5991,.F.);
#8005=ORIENTED_EDGE('',*,*,#5988,.F.);
#8006=ORIENTED_EDGE('',*,*,#6000,.F.);
#8007=ORIENTED_EDGE('',*,*,#6001,.T.);
#8008=ORIENTED_EDGE('',*,*,#5999,.T.);
#8009=ORIENTED_EDGE('',*,*,#6001,.F.);
#8010=ORIENTED_EDGE('',*,*,#5998,.T.);
#8011=ORIENTED_EDGE('',*,*,#6002,.T.);
#8012=ORIENTED_EDGE('',*,*,#6003,.T.);
#8013=ORIENTED_EDGE('',*,*,#6002,.F.);
#8014=ORIENTED_EDGE('',*,*,#6000,.T.);
#8015=ORIENTED_EDGE('',*,*,#5997,.T.);
#8016=ORIENTED_EDGE('',*,*,#5987,.T.);
#8017=ORIENTED_EDGE('',*,*,#5979,.T.);
#8018=ORIENTED_EDGE('',*,*,#5969,.T.);
#8019=ORIENTED_EDGE('',*,*,#5961,.T.);
#8020=ORIENTED_EDGE('',*,*,#5990,.F.);
#8021=ORIENTED_EDGE('',*,*,#6003,.F.);
#8022=ORIENTED_EDGE('',*,*,#6004,.F.);
#8023=ORIENTED_EDGE('',*,*,#6005,.T.);
#8024=ORIENTED_EDGE('',*,*,#6006,.F.);
#8025=ORIENTED_EDGE('',*,*,#6007,.F.);
#8026=ORIENTED_EDGE('',*,*,#6008,.T.);
#8027=ORIENTED_EDGE('',*,*,#6009,.F.);
#8028=ORIENTED_EDGE('',*,*,#6008,.F.);
#8029=ORIENTED_EDGE('',*,*,#6010,.F.);
#8030=ORIENTED_EDGE('',*,*,#6011,.F.);
#8031=ORIENTED_EDGE('',*,*,#6005,.F.);
#8032=ORIENTED_EDGE('',*,*,#6012,.F.);
#8033=ORIENTED_EDGE('',*,*,#6013,.T.);
#8034=ORIENTED_EDGE('',*,*,#6014,.F.);
#8035=ORIENTED_EDGE('',*,*,#6015,.F.);
#8036=ORIENTED_EDGE('',*,*,#6016,.T.);
#8037=ORIENTED_EDGE('',*,*,#6017,.F.);
#8038=ORIENTED_EDGE('',*,*,#6016,.F.);
#8039=ORIENTED_EDGE('',*,*,#6018,.F.);
#8040=ORIENTED_EDGE('',*,*,#6019,.F.);
#8041=ORIENTED_EDGE('',*,*,#6013,.F.);
#8042=ORIENTED_EDGE('',*,*,#6020,.F.);
#8043=ORIENTED_EDGE('',*,*,#6021,.T.);
#8044=ORIENTED_EDGE('',*,*,#6022,.T.);
#8045=ORIENTED_EDGE('',*,*,#6023,.F.);
#8046=ORIENTED_EDGE('',*,*,#6024,.F.);
#8047=ORIENTED_EDGE('',*,*,#6025,.F.);
#8048=ORIENTED_EDGE('',*,*,#6022,.F.);
#8049=ORIENTED_EDGE('',*,*,#6026,.T.);
#8050=ORIENTED_EDGE('',*,*,#6027,.F.);
#8051=ORIENTED_EDGE('',*,*,#6026,.F.);
#8052=ORIENTED_EDGE('',*,*,#6021,.F.);
#8053=ORIENTED_EDGE('',*,*,#6028,.F.);
#8054=ORIENTED_EDGE('',*,*,#6029,.T.);
#8055=ORIENTED_EDGE('',*,*,#6030,.T.);
#8056=ORIENTED_EDGE('',*,*,#6031,.F.);
#8057=ORIENTED_EDGE('',*,*,#6032,.F.);
#8058=ORIENTED_EDGE('',*,*,#6033,.F.);
#8059=ORIENTED_EDGE('',*,*,#6030,.F.);
#8060=ORIENTED_EDGE('',*,*,#6034,.T.);
#8061=ORIENTED_EDGE('',*,*,#6035,.F.);
#8062=ORIENTED_EDGE('',*,*,#6034,.F.);
#8063=ORIENTED_EDGE('',*,*,#6029,.F.);
#8064=ORIENTED_EDGE('',*,*,#6006,.T.);
#8065=ORIENTED_EDGE('',*,*,#6004,.T.);
#8066=ORIENTED_EDGE('',*,*,#6011,.T.);
#8067=ORIENTED_EDGE('',*,*,#6036,.T.);
#8068=ORIENTED_EDGE('',*,*,#6037,.T.);
#8069=ORIENTED_EDGE('',*,*,#6038,.T.);
#8070=ORIENTED_EDGE('',*,*,#6037,.F.);
#8071=ORIENTED_EDGE('',*,*,#6039,.T.);
#8072=ORIENTED_EDGE('',*,*,#6014,.T.);
#8073=ORIENTED_EDGE('',*,*,#6012,.T.);
#8074=ORIENTED_EDGE('',*,*,#6019,.T.);
#8075=ORIENTED_EDGE('',*,*,#6040,.T.);
#8076=ORIENTED_EDGE('',*,*,#6023,.T.);
#8077=ORIENTED_EDGE('',*,*,#6020,.T.);
#8078=ORIENTED_EDGE('',*,*,#6025,.T.);
#8079=ORIENTED_EDGE('',*,*,#6041,.T.);
#8080=ORIENTED_EDGE('',*,*,#6031,.T.);
#8081=ORIENTED_EDGE('',*,*,#6028,.T.);
#8082=ORIENTED_EDGE('',*,*,#6033,.T.);
#8083=ORIENTED_EDGE('',*,*,#6042,.T.);
#8084=ORIENTED_EDGE('',*,*,#6043,.F.);
#8085=ORIENTED_EDGE('',*,*,#6044,.T.);
#8086=ORIENTED_EDGE('',*,*,#6045,.F.);
#8087=ORIENTED_EDGE('',*,*,#6044,.F.);
#8088=ORIENTED_EDGE('',*,*,#6043,.T.);
#8089=ORIENTED_EDGE('',*,*,#6046,.F.);
#8090=ORIENTED_EDGE('',*,*,#6047,.F.);
#8091=ORIENTED_EDGE('',*,*,#6010,.T.);
#8092=ORIENTED_EDGE('',*,*,#6007,.T.);
#8093=ORIENTED_EDGE('',*,*,#6042,.F.);
#8094=ORIENTED_EDGE('',*,*,#6032,.T.);
#8095=ORIENTED_EDGE('',*,*,#6041,.F.);
#8096=ORIENTED_EDGE('',*,*,#6024,.T.);
#8097=ORIENTED_EDGE('',*,*,#6040,.F.);
#8098=ORIENTED_EDGE('',*,*,#6018,.T.);
#8099=ORIENTED_EDGE('',*,*,#6015,.T.);
#8100=ORIENTED_EDGE('',*,*,#6039,.F.);
#8101=ORIENTED_EDGE('',*,*,#6036,.F.);
#8102=ORIENTED_EDGE('',*,*,#6048,.F.);
#8103=ORIENTED_EDGE('',*,*,#6049,.T.);
#8104=ORIENTED_EDGE('',*,*,#6047,.T.);
#8105=ORIENTED_EDGE('',*,*,#6049,.F.);
#8106=ORIENTED_EDGE('',*,*,#6046,.T.);
#8107=ORIENTED_EDGE('',*,*,#6050,.T.);
#8108=ORIENTED_EDGE('',*,*,#6051,.T.);
#8109=ORIENTED_EDGE('',*,*,#6050,.F.);
#8110=ORIENTED_EDGE('',*,*,#6048,.T.);
#8111=ORIENTED_EDGE('',*,*,#6045,.T.);
#8112=ORIENTED_EDGE('',*,*,#6035,.T.);
#8113=ORIENTED_EDGE('',*,*,#6027,.T.);
#8114=ORIENTED_EDGE('',*,*,#6017,.T.);
#8115=ORIENTED_EDGE('',*,*,#6009,.T.);
#8116=ORIENTED_EDGE('',*,*,#6038,.F.);
#8117=ORIENTED_EDGE('',*,*,#6051,.F.);
#8118=ORIENTED_EDGE('',*,*,#6052,.F.);
#8119=ORIENTED_EDGE('',*,*,#6053,.T.);
#8120=ORIENTED_EDGE('',*,*,#6054,.F.);
#8121=ORIENTED_EDGE('',*,*,#6055,.F.);
#8122=ORIENTED_EDGE('',*,*,#6056,.T.);
#8123=ORIENTED_EDGE('',*,*,#6057,.F.);
#8124=ORIENTED_EDGE('',*,*,#6056,.F.);
#8125=ORIENTED_EDGE('',*,*,#6058,.F.);
#8126=ORIENTED_EDGE('',*,*,#6059,.F.);
#8127=ORIENTED_EDGE('',*,*,#6053,.F.);
#8128=ORIENTED_EDGE('',*,*,#6060,.F.);
#8129=ORIENTED_EDGE('',*,*,#6061,.T.);
#8130=ORIENTED_EDGE('',*,*,#6062,.F.);
#8131=ORIENTED_EDGE('',*,*,#6063,.F.);
#8132=ORIENTED_EDGE('',*,*,#6064,.T.);
#8133=ORIENTED_EDGE('',*,*,#6065,.F.);
#8134=ORIENTED_EDGE('',*,*,#6064,.F.);
#8135=ORIENTED_EDGE('',*,*,#6066,.F.);
#8136=ORIENTED_EDGE('',*,*,#6067,.F.);
#8137=ORIENTED_EDGE('',*,*,#6061,.F.);
#8138=ORIENTED_EDGE('',*,*,#6068,.F.);
#8139=ORIENTED_EDGE('',*,*,#6069,.T.);
#8140=ORIENTED_EDGE('',*,*,#6070,.T.);
#8141=ORIENTED_EDGE('',*,*,#6071,.F.);
#8142=ORIENTED_EDGE('',*,*,#6072,.F.);
#8143=ORIENTED_EDGE('',*,*,#6073,.F.);
#8144=ORIENTED_EDGE('',*,*,#6070,.F.);
#8145=ORIENTED_EDGE('',*,*,#6074,.T.);
#8146=ORIENTED_EDGE('',*,*,#6075,.F.);
#8147=ORIENTED_EDGE('',*,*,#6074,.F.);
#8148=ORIENTED_EDGE('',*,*,#6069,.F.);
#8149=ORIENTED_EDGE('',*,*,#6076,.F.);
#8150=ORIENTED_EDGE('',*,*,#6077,.T.);
#8151=ORIENTED_EDGE('',*,*,#6078,.T.);
#8152=ORIENTED_EDGE('',*,*,#6079,.F.);
#8153=ORIENTED_EDGE('',*,*,#6080,.F.);
#8154=ORIENTED_EDGE('',*,*,#6081,.F.);
#8155=ORIENTED_EDGE('',*,*,#6078,.F.);
#8156=ORIENTED_EDGE('',*,*,#6082,.T.);
#8157=ORIENTED_EDGE('',*,*,#6083,.F.);
#8158=ORIENTED_EDGE('',*,*,#6082,.F.);
#8159=ORIENTED_EDGE('',*,*,#6077,.F.);
#8160=ORIENTED_EDGE('',*,*,#6054,.T.);
#8161=ORIENTED_EDGE('',*,*,#6052,.T.);
#8162=ORIENTED_EDGE('',*,*,#6059,.T.);
#8163=ORIENTED_EDGE('',*,*,#6084,.T.);
#8164=ORIENTED_EDGE('',*,*,#6085,.T.);
#8165=ORIENTED_EDGE('',*,*,#6086,.T.);
#8166=ORIENTED_EDGE('',*,*,#6085,.F.);
#8167=ORIENTED_EDGE('',*,*,#6087,.T.);
#8168=ORIENTED_EDGE('',*,*,#6062,.T.);
#8169=ORIENTED_EDGE('',*,*,#6060,.T.);
#8170=ORIENTED_EDGE('',*,*,#6067,.T.);
#8171=ORIENTED_EDGE('',*,*,#6088,.T.);
#8172=ORIENTED_EDGE('',*,*,#6071,.T.);
#8173=ORIENTED_EDGE('',*,*,#6068,.T.);
#8174=ORIENTED_EDGE('',*,*,#6073,.T.);
#8175=ORIENTED_EDGE('',*,*,#6089,.T.);
#8176=ORIENTED_EDGE('',*,*,#6079,.T.);
#8177=ORIENTED_EDGE('',*,*,#6076,.T.);
#8178=ORIENTED_EDGE('',*,*,#6081,.T.);
#8179=ORIENTED_EDGE('',*,*,#6090,.T.);
#8180=ORIENTED_EDGE('',*,*,#6091,.F.);
#8181=ORIENTED_EDGE('',*,*,#6092,.T.);
#8182=ORIENTED_EDGE('',*,*,#6093,.F.);
#8183=ORIENTED_EDGE('',*,*,#6092,.F.);
#8184=ORIENTED_EDGE('',*,*,#6091,.T.);
#8185=ORIENTED_EDGE('',*,*,#6094,.F.);
#8186=ORIENTED_EDGE('',*,*,#6095,.F.);
#8187=ORIENTED_EDGE('',*,*,#6058,.T.);
#8188=ORIENTED_EDGE('',*,*,#6055,.T.);
#8189=ORIENTED_EDGE('',*,*,#6090,.F.);
#8190=ORIENTED_EDGE('',*,*,#6080,.T.);
#8191=ORIENTED_EDGE('',*,*,#6089,.F.);
#8192=ORIENTED_EDGE('',*,*,#6072,.T.);
#8193=ORIENTED_EDGE('',*,*,#6088,.F.);
#8194=ORIENTED_EDGE('',*,*,#6066,.T.);
#8195=ORIENTED_EDGE('',*,*,#6063,.T.);
#8196=ORIENTED_EDGE('',*,*,#6087,.F.);
#8197=ORIENTED_EDGE('',*,*,#6084,.F.);
#8198=ORIENTED_EDGE('',*,*,#6096,.F.);
#8199=ORIENTED_EDGE('',*,*,#6097,.T.);
#8200=ORIENTED_EDGE('',*,*,#6095,.T.);
#8201=ORIENTED_EDGE('',*,*,#6097,.F.);
#8202=ORIENTED_EDGE('',*,*,#6094,.T.);
#8203=ORIENTED_EDGE('',*,*,#6098,.T.);
#8204=ORIENTED_EDGE('',*,*,#6099,.T.);
#8205=ORIENTED_EDGE('',*,*,#6098,.F.);
#8206=ORIENTED_EDGE('',*,*,#6096,.T.);
#8207=ORIENTED_EDGE('',*,*,#6093,.T.);
#8208=ORIENTED_EDGE('',*,*,#6083,.T.);
#8209=ORIENTED_EDGE('',*,*,#6075,.T.);
#8210=ORIENTED_EDGE('',*,*,#6065,.T.);
#8211=ORIENTED_EDGE('',*,*,#6057,.T.);
#8212=ORIENTED_EDGE('',*,*,#6086,.F.);
#8213=ORIENTED_EDGE('',*,*,#6099,.F.);
#8214=ORIENTED_EDGE('',*,*,#6100,.F.);
#8215=ORIENTED_EDGE('',*,*,#6101,.T.);
#8216=ORIENTED_EDGE('',*,*,#6102,.F.);
#8217=ORIENTED_EDGE('',*,*,#6103,.F.);
#8218=ORIENTED_EDGE('',*,*,#6104,.T.);
#8219=ORIENTED_EDGE('',*,*,#6105,.F.);
#8220=ORIENTED_EDGE('',*,*,#6104,.F.);
#8221=ORIENTED_EDGE('',*,*,#6106,.F.);
#8222=ORIENTED_EDGE('',*,*,#6107,.F.);
#8223=ORIENTED_EDGE('',*,*,#6101,.F.);
#8224=ORIENTED_EDGE('',*,*,#6108,.F.);
#8225=ORIENTED_EDGE('',*,*,#6109,.T.);
#8226=ORIENTED_EDGE('',*,*,#6110,.F.);
#8227=ORIENTED_EDGE('',*,*,#6111,.F.);
#8228=ORIENTED_EDGE('',*,*,#6112,.T.);
#8229=ORIENTED_EDGE('',*,*,#6113,.F.);
#8230=ORIENTED_EDGE('',*,*,#6112,.F.);
#8231=ORIENTED_EDGE('',*,*,#6114,.F.);
#8232=ORIENTED_EDGE('',*,*,#6115,.F.);
#8233=ORIENTED_EDGE('',*,*,#6109,.F.);
#8234=ORIENTED_EDGE('',*,*,#6116,.F.);
#8235=ORIENTED_EDGE('',*,*,#6117,.T.);
#8236=ORIENTED_EDGE('',*,*,#6118,.T.);
#8237=ORIENTED_EDGE('',*,*,#6119,.F.);
#8238=ORIENTED_EDGE('',*,*,#6120,.F.);
#8239=ORIENTED_EDGE('',*,*,#6121,.F.);
#8240=ORIENTED_EDGE('',*,*,#6118,.F.);
#8241=ORIENTED_EDGE('',*,*,#6122,.T.);
#8242=ORIENTED_EDGE('',*,*,#6123,.F.);
#8243=ORIENTED_EDGE('',*,*,#6122,.F.);
#8244=ORIENTED_EDGE('',*,*,#6117,.F.);
#8245=ORIENTED_EDGE('',*,*,#6124,.F.);
#8246=ORIENTED_EDGE('',*,*,#6125,.T.);
#8247=ORIENTED_EDGE('',*,*,#6126,.T.);
#8248=ORIENTED_EDGE('',*,*,#6127,.F.);
#8249=ORIENTED_EDGE('',*,*,#6128,.F.);
#8250=ORIENTED_EDGE('',*,*,#6129,.F.);
#8251=ORIENTED_EDGE('',*,*,#6126,.F.);
#8252=ORIENTED_EDGE('',*,*,#6130,.T.);
#8253=ORIENTED_EDGE('',*,*,#6131,.F.);
#8254=ORIENTED_EDGE('',*,*,#6130,.F.);
#8255=ORIENTED_EDGE('',*,*,#6125,.F.);
#8256=ORIENTED_EDGE('',*,*,#6102,.T.);
#8257=ORIENTED_EDGE('',*,*,#6100,.T.);
#8258=ORIENTED_EDGE('',*,*,#6107,.T.);
#8259=ORIENTED_EDGE('',*,*,#6132,.T.);
#8260=ORIENTED_EDGE('',*,*,#6133,.T.);
#8261=ORIENTED_EDGE('',*,*,#6134,.T.);
#8262=ORIENTED_EDGE('',*,*,#6133,.F.);
#8263=ORIENTED_EDGE('',*,*,#6135,.T.);
#8264=ORIENTED_EDGE('',*,*,#6110,.T.);
#8265=ORIENTED_EDGE('',*,*,#6108,.T.);
#8266=ORIENTED_EDGE('',*,*,#6115,.T.);
#8267=ORIENTED_EDGE('',*,*,#6136,.T.);
#8268=ORIENTED_EDGE('',*,*,#6119,.T.);
#8269=ORIENTED_EDGE('',*,*,#6116,.T.);
#8270=ORIENTED_EDGE('',*,*,#6121,.T.);
#8271=ORIENTED_EDGE('',*,*,#6137,.T.);
#8272=ORIENTED_EDGE('',*,*,#6127,.T.);
#8273=ORIENTED_EDGE('',*,*,#6124,.T.);
#8274=ORIENTED_EDGE('',*,*,#6129,.T.);
#8275=ORIENTED_EDGE('',*,*,#6138,.T.);
#8276=ORIENTED_EDGE('',*,*,#6139,.F.);
#8277=ORIENTED_EDGE('',*,*,#6140,.T.);
#8278=ORIENTED_EDGE('',*,*,#6141,.F.);
#8279=ORIENTED_EDGE('',*,*,#6140,.F.);
#8280=ORIENTED_EDGE('',*,*,#6139,.T.);
#8281=ORIENTED_EDGE('',*,*,#6142,.F.);
#8282=ORIENTED_EDGE('',*,*,#6143,.F.);
#8283=ORIENTED_EDGE('',*,*,#6106,.T.);
#8284=ORIENTED_EDGE('',*,*,#6103,.T.);
#8285=ORIENTED_EDGE('',*,*,#6138,.F.);
#8286=ORIENTED_EDGE('',*,*,#6128,.T.);
#8287=ORIENTED_EDGE('',*,*,#6137,.F.);
#8288=ORIENTED_EDGE('',*,*,#6120,.T.);
#8289=ORIENTED_EDGE('',*,*,#6136,.F.);
#8290=ORIENTED_EDGE('',*,*,#6114,.T.);
#8291=ORIENTED_EDGE('',*,*,#6111,.T.);
#8292=ORIENTED_EDGE('',*,*,#6135,.F.);
#8293=ORIENTED_EDGE('',*,*,#6132,.F.);
#8294=ORIENTED_EDGE('',*,*,#6144,.F.);
#8295=ORIENTED_EDGE('',*,*,#6145,.T.);
#8296=ORIENTED_EDGE('',*,*,#6143,.T.);
#8297=ORIENTED_EDGE('',*,*,#6145,.F.);
#8298=ORIENTED_EDGE('',*,*,#6142,.T.);
#8299=ORIENTED_EDGE('',*,*,#6146,.T.);
#8300=ORIENTED_EDGE('',*,*,#6147,.T.);
#8301=ORIENTED_EDGE('',*,*,#6146,.F.);
#8302=ORIENTED_EDGE('',*,*,#6144,.T.);
#8303=ORIENTED_EDGE('',*,*,#6141,.T.);
#8304=ORIENTED_EDGE('',*,*,#6131,.T.);
#8305=ORIENTED_EDGE('',*,*,#6123,.T.);
#8306=ORIENTED_EDGE('',*,*,#6113,.T.);
#8307=ORIENTED_EDGE('',*,*,#6105,.T.);
#8308=ORIENTED_EDGE('',*,*,#6134,.F.);
#8309=ORIENTED_EDGE('',*,*,#6147,.F.);
#8310=ORIENTED_EDGE('',*,*,#6148,.F.);
#8311=ORIENTED_EDGE('',*,*,#6149,.T.);
#8312=ORIENTED_EDGE('',*,*,#6150,.F.);
#8313=ORIENTED_EDGE('',*,*,#6149,.F.);
#8314=ORIENTED_EDGE('',*,*,#6151,.F.);
#8315=ORIENTED_EDGE('',*,*,#6152,.T.);
#8316=ORIENTED_EDGE('',*,*,#6153,.F.);
#8317=ORIENTED_EDGE('',*,*,#6152,.F.);
#8318=ORIENTED_EDGE('',*,*,#6154,.F.);
#8319=ORIENTED_EDGE('',*,*,#6155,.T.);
#8320=ORIENTED_EDGE('',*,*,#6156,.F.);
#8321=ORIENTED_EDGE('',*,*,#6155,.F.);
#8322=ORIENTED_EDGE('',*,*,#6157,.F.);
#8323=ORIENTED_EDGE('',*,*,#6158,.T.);
#8324=ORIENTED_EDGE('',*,*,#6159,.F.);
#8325=ORIENTED_EDGE('',*,*,#6158,.F.);
#8326=ORIENTED_EDGE('',*,*,#6160,.F.);
#8327=ORIENTED_EDGE('',*,*,#6161,.F.);
#8328=ORIENTED_EDGE('',*,*,#6157,.T.);
#8329=ORIENTED_EDGE('',*,*,#6154,.T.);
#8330=ORIENTED_EDGE('',*,*,#6151,.T.);
#8331=ORIENTED_EDGE('',*,*,#6148,.T.);
#8332=ORIENTED_EDGE('',*,*,#6162,.F.);
#8333=ORIENTED_EDGE('',*,*,#6163,.T.);
#8334=ORIENTED_EDGE('',*,*,#6160,.T.);
#8335=ORIENTED_EDGE('',*,*,#6163,.F.);
#8336=ORIENTED_EDGE('',*,*,#6161,.T.);
#8337=ORIENTED_EDGE('',*,*,#6164,.T.);
#8338=ORIENTED_EDGE('',*,*,#6165,.T.);
#8339=ORIENTED_EDGE('',*,*,#6164,.F.);
#8340=ORIENTED_EDGE('',*,*,#6162,.T.);
#8341=ORIENTED_EDGE('',*,*,#6150,.T.);
#8342=ORIENTED_EDGE('',*,*,#6153,.T.);
#8343=ORIENTED_EDGE('',*,*,#6156,.T.);
#8344=ORIENTED_EDGE('',*,*,#6159,.T.);
#8345=ORIENTED_EDGE('',*,*,#6165,.F.);
#8346=ORIENTED_EDGE('',*,*,#6166,.F.);
#8347=ORIENTED_EDGE('',*,*,#6167,.F.);
#8348=ORIENTED_EDGE('',*,*,#6168,.F.);
#8349=ORIENTED_EDGE('',*,*,#6169,.F.);
#8350=ORIENTED_EDGE('',*,*,#6170,.F.);
#8351=ORIENTED_EDGE('',*,*,#6169,.T.);
#8352=ORIENTED_EDGE('',*,*,#6171,.F.);
#8353=ORIENTED_EDGE('',*,*,#6172,.T.);
#8354=ORIENTED_EDGE('',*,*,#6173,.F.);
#8355=ORIENTED_EDGE('',*,*,#6172,.F.);
#8356=ORIENTED_EDGE('',*,*,#6174,.F.);
#8357=ORIENTED_EDGE('',*,*,#6175,.F.);
#8358=ORIENTED_EDGE('',*,*,#6176,.F.);
#8359=ORIENTED_EDGE('',*,*,#6175,.T.);
#8360=ORIENTED_EDGE('',*,*,#6177,.T.);
#8361=ORIENTED_EDGE('',*,*,#6167,.T.);
#8362=ORIENTED_EDGE('',*,*,#6177,.F.);
#8363=ORIENTED_EDGE('',*,*,#6174,.T.);
#8364=ORIENTED_EDGE('',*,*,#6171,.T.);
#8365=ORIENTED_EDGE('',*,*,#6168,.T.);
#8366=ORIENTED_EDGE('',*,*,#6178,.F.);
#8367=ORIENTED_EDGE('',*,*,#6179,.T.);
#8368=ORIENTED_EDGE('',*,*,#6180,.F.);
#8369=ORIENTED_EDGE('',*,*,#6181,.T.);
#8370=ORIENTED_EDGE('',*,*,#6178,.T.);
#8371=ORIENTED_EDGE('',*,*,#6181,.F.);
#8372=ORIENTED_EDGE('',*,*,#6180,.T.);
#8373=ORIENTED_EDGE('',*,*,#6182,.F.);
#8374=ORIENTED_EDGE('',*,*,#6183,.F.);
#8375=ORIENTED_EDGE('',*,*,#6184,.T.);
#8376=ORIENTED_EDGE('',*,*,#6182,.T.);
#8377=ORIENTED_EDGE('',*,*,#6184,.F.);
#8378=ORIENTED_EDGE('',*,*,#6185,.F.);
#8379=ORIENTED_EDGE('',*,*,#6183,.T.);
#8380=ORIENTED_EDGE('',*,*,#6186,.F.);
#8381=ORIENTED_EDGE('',*,*,#6187,.T.);
#8382=ORIENTED_EDGE('',*,*,#6185,.T.);
#8383=ORIENTED_EDGE('',*,*,#6187,.F.);
#8384=ORIENTED_EDGE('',*,*,#6186,.T.);
#8385=ORIENTED_EDGE('',*,*,#6188,.F.);
#8386=ORIENTED_EDGE('',*,*,#6189,.F.);
#8387=ORIENTED_EDGE('',*,*,#6190,.T.);
#8388=ORIENTED_EDGE('',*,*,#6188,.T.);
#8389=ORIENTED_EDGE('',*,*,#6190,.F.);
#8390=ORIENTED_EDGE('',*,*,#6191,.F.);
#8391=ORIENTED_EDGE('',*,*,#6189,.T.);
#8392=ORIENTED_EDGE('',*,*,#6192,.F.);
#8393=ORIENTED_EDGE('',*,*,#6193,.T.);
#8394=ORIENTED_EDGE('',*,*,#6191,.T.);
#8395=ORIENTED_EDGE('',*,*,#6193,.F.);
#8396=ORIENTED_EDGE('',*,*,#6192,.T.);
#8397=ORIENTED_EDGE('',*,*,#6194,.F.);
#8398=ORIENTED_EDGE('',*,*,#6194,.T.);
#8399=ORIENTED_EDGE('',*,*,#6195,.T.);
#8400=ORIENTED_EDGE('',*,*,#6179,.F.);
#8401=ORIENTED_EDGE('',*,*,#6195,.F.);
#8402=ORIENTED_EDGE('',*,*,#6173,.T.);
#8403=ORIENTED_EDGE('',*,*,#6176,.T.);
#8404=ORIENTED_EDGE('',*,*,#6166,.T.);
#8405=ORIENTED_EDGE('',*,*,#6170,.T.);
#8406=ORIENTED_EDGE('',*,*,#6196,.F.);
#8407=ORIENTED_EDGE('',*,*,#6197,.F.);
#8408=ORIENTED_EDGE('',*,*,#6198,.F.);
#8409=ORIENTED_EDGE('',*,*,#6199,.F.);
#8410=ORIENTED_EDGE('',*,*,#6200,.F.);
#8411=ORIENTED_EDGE('',*,*,#6199,.T.);
#8412=ORIENTED_EDGE('',*,*,#6201,.F.);
#8413=ORIENTED_EDGE('',*,*,#6202,.T.);
#8414=ORIENTED_EDGE('',*,*,#6203,.F.);
#8415=ORIENTED_EDGE('',*,*,#6202,.F.);
#8416=ORIENTED_EDGE('',*,*,#6204,.F.);
#8417=ORIENTED_EDGE('',*,*,#6205,.F.);
#8418=ORIENTED_EDGE('',*,*,#6206,.F.);
#8419=ORIENTED_EDGE('',*,*,#6205,.T.);
#8420=ORIENTED_EDGE('',*,*,#6207,.F.);
#8421=ORIENTED_EDGE('',*,*,#6197,.T.);
#8422=ORIENTED_EDGE('',*,*,#6208,.F.);
#8423=ORIENTED_EDGE('',*,*,#6209,.T.);
#8424=ORIENTED_EDGE('',*,*,#6210,.F.);
#8425=ORIENTED_EDGE('',*,*,#6211,.T.);
#8426=ORIENTED_EDGE('',*,*,#6208,.T.);
#8427=ORIENTED_EDGE('',*,*,#6211,.F.);
#8428=ORIENTED_EDGE('',*,*,#6203,.T.);
#8429=ORIENTED_EDGE('',*,*,#6206,.T.);
#8430=ORIENTED_EDGE('',*,*,#6196,.T.);
#8431=ORIENTED_EDGE('',*,*,#6200,.T.);
#8432=ORIENTED_EDGE('',*,*,#6210,.T.);
#8433=ORIENTED_EDGE('',*,*,#6212,.F.);
#8434=ORIENTED_EDGE('',*,*,#6212,.T.);
#8435=ORIENTED_EDGE('',*,*,#6213,.T.);
#8436=ORIENTED_EDGE('',*,*,#6209,.F.);
#8437=ORIENTED_EDGE('',*,*,#6213,.F.);
#8438=ORIENTED_EDGE('',*,*,#6204,.T.);
#8439=ORIENTED_EDGE('',*,*,#6201,.T.);
#8440=ORIENTED_EDGE('',*,*,#6198,.T.);
#8441=ORIENTED_EDGE('',*,*,#6207,.T.);
#8442=ORIENTED_EDGE('',*,*,#6214,.F.);
#8443=ORIENTED_EDGE('',*,*,#6215,.F.);
#8444=ORIENTED_EDGE('',*,*,#6216,.T.);
#8445=ORIENTED_EDGE('',*,*,#6214,.T.);
#8446=ORIENTED_EDGE('',*,*,#6216,.F.);
#8447=ORIENTED_EDGE('',*,*,#6217,.F.);
#8448=ORIENTED_EDGE('',*,*,#6218,.T.);
#8449=ORIENTED_EDGE('',*,*,#6215,.T.);
#8450=ORIENTED_EDGE('',*,*,#6218,.F.);
#8451=ORIENTED_EDGE('',*,*,#6219,.F.);
#8452=ORIENTED_EDGE('',*,*,#6220,.T.);
#8453=ORIENTED_EDGE('',*,*,#6217,.T.);
#8454=ORIENTED_EDGE('',*,*,#6220,.F.);
#8455=ORIENTED_EDGE('',*,*,#6219,.T.);
#8456=ORIENTED_EDGE('',*,*,#6221,.F.);
#8457=ORIENTED_EDGE('',*,*,#6222,.F.);
#8458=ORIENTED_EDGE('',*,*,#6223,.T.);
#8459=ORIENTED_EDGE('',*,*,#6221,.T.);
#8460=ORIENTED_EDGE('',*,*,#6223,.F.);
#8461=ORIENTED_EDGE('',*,*,#6224,.F.);
#8462=ORIENTED_EDGE('',*,*,#6225,.T.);
#8463=ORIENTED_EDGE('',*,*,#6222,.T.);
#8464=ORIENTED_EDGE('',*,*,#6225,.F.);
#8465=ORIENTED_EDGE('',*,*,#6226,.F.);
#8466=ORIENTED_EDGE('',*,*,#6227,.T.);
#8467=ORIENTED_EDGE('',*,*,#6224,.T.);
#8468=ORIENTED_EDGE('',*,*,#6227,.F.);
#8469=ORIENTED_EDGE('',*,*,#6226,.T.);
#8470=ORIENTED_EDGE('',*,*,#6228,.T.);
#8471=ORIENTED_EDGE('',*,*,#6229,.T.);
#8472=ORIENTED_EDGE('',*,*,#6230,.T.);
#8473=ORIENTED_EDGE('',*,*,#6231,.F.);
#8474=ORIENTED_EDGE('',*,*,#6232,.T.);
#8475=ORIENTED_EDGE('',*,*,#6233,.T.);
#8476=ORIENTED_EDGE('',*,*,#6234,.T.);
#8477=ORIENTED_EDGE('',*,*,#6229,.F.);
#8478=ORIENTED_EDGE('',*,*,#6235,.T.);
#8479=ORIENTED_EDGE('',*,*,#6236,.T.);
#8480=ORIENTED_EDGE('',*,*,#6237,.T.);
#8481=ORIENTED_EDGE('',*,*,#6233,.F.);
#8482=ORIENTED_EDGE('',*,*,#6238,.T.);
#8483=ORIENTED_EDGE('',*,*,#6239,.T.);
#8484=ORIENTED_EDGE('',*,*,#6240,.T.);
#8485=ORIENTED_EDGE('',*,*,#6236,.F.);
#8486=ORIENTED_EDGE('',*,*,#6241,.T.);
#8487=ORIENTED_EDGE('',*,*,#6242,.T.);
#8488=ORIENTED_EDGE('',*,*,#6243,.T.);
#8489=ORIENTED_EDGE('',*,*,#6239,.F.);
#8490=ORIENTED_EDGE('',*,*,#6244,.T.);
#8491=ORIENTED_EDGE('',*,*,#6231,.T.);
#8492=ORIENTED_EDGE('',*,*,#6245,.T.);
#8493=ORIENTED_EDGE('',*,*,#6242,.F.);
#8494=ORIENTED_EDGE('',*,*,#6244,.F.);
#8495=ORIENTED_EDGE('',*,*,#6241,.F.);
#8496=ORIENTED_EDGE('',*,*,#6238,.F.);
#8497=ORIENTED_EDGE('',*,*,#6235,.F.);
#8498=ORIENTED_EDGE('',*,*,#6232,.F.);
#8499=ORIENTED_EDGE('',*,*,#6228,.F.);
#8500=ORIENTED_EDGE('',*,*,#6245,.F.);
#8501=ORIENTED_EDGE('',*,*,#6230,.F.);
#8502=ORIENTED_EDGE('',*,*,#6234,.F.);
#8503=ORIENTED_EDGE('',*,*,#6237,.F.);
#8504=ORIENTED_EDGE('',*,*,#6240,.F.);
#8505=ORIENTED_EDGE('',*,*,#6243,.F.);
#8506=CYLINDRICAL_SURFACE('',#9763,0.275);
#8507=CYLINDRICAL_SURFACE('',#9766,0.275);
#8508=CYLINDRICAL_SURFACE('',#9769,0.5);
#8509=CYLINDRICAL_SURFACE('',#9772,0.5);
#8510=CYLINDRICAL_SURFACE('',#9775,0.5);
#8511=CYLINDRICAL_SURFACE('',#9778,0.5);
#8512=CYLINDRICAL_SURFACE('',#9781,0.21);
#8513=CYLINDRICAL_SURFACE('',#9784,0.21);
#8514=CYLINDRICAL_SURFACE('',#9787,0.21);
#8515=CYLINDRICAL_SURFACE('',#9790,0.21);
#8516=CYLINDRICAL_SURFACE('',#9793,0.275);
#8517=CYLINDRICAL_SURFACE('',#9796,0.275);
#8518=CYLINDRICAL_SURFACE('',#9799,0.275);
#8519=CYLINDRICAL_SURFACE('',#9802,0.275);
#8520=CYLINDRICAL_SURFACE('',#9805,0.275);
#8521=CYLINDRICAL_SURFACE('',#9808,0.275);
#8522=CYLINDRICAL_SURFACE('',#9811,0.275);
#8523=CYLINDRICAL_SURFACE('',#9814,0.275);
#8524=CYLINDRICAL_SURFACE('',#9817,0.275);
#8525=CYLINDRICAL_SURFACE('',#9820,0.275);
#8526=CYLINDRICAL_SURFACE('',#9823,0.275);
#8527=CYLINDRICAL_SURFACE('',#9826,0.275);
#8528=CYLINDRICAL_SURFACE('',#9850,0.275);
#8529=CYLINDRICAL_SURFACE('',#9853,0.275);
#8530=CYLINDRICAL_SURFACE('',#9856,0.275);
#8531=CYLINDRICAL_SURFACE('',#9859,0.275);
#8532=CYLINDRICAL_SURFACE('',#9862,0.275);
#8533=CYLINDRICAL_SURFACE('',#9865,0.275);
#8534=CYLINDRICAL_SURFACE('',#9868,0.275);
#8535=CYLINDRICAL_SURFACE('',#9871,0.275);
#8536=CYLINDRICAL_SURFACE('',#9874,0.275);
#8537=CYLINDRICAL_SURFACE('',#9877,0.275);
#8538=CYLINDRICAL_SURFACE('',#9880,0.275);
#8539=CYLINDRICAL_SURFACE('',#9883,0.275);
#8540=CYLINDRICAL_SURFACE('',#9886,0.275);
#8541=CYLINDRICAL_SURFACE('',#9889,0.275);
#8542=CYLINDRICAL_SURFACE('',#9892,0.61);
#8543=CYLINDRICAL_SURFACE('',#9895,0.61);
#8544=CYLINDRICAL_SURFACE('',#9898,0.61);
#8545=CYLINDRICAL_SURFACE('',#9901,0.61);
#8546=CYLINDRICAL_SURFACE('',#9911,0.210000000000001);
#8547=CYLINDRICAL_SURFACE('',#9915,0.210000000000001);
#8548=CYLINDRICAL_SURFACE('',#9919,0.210000000000001);
#8549=CYLINDRICAL_SURFACE('',#9923,0.210000000000001);
#8550=CYLINDRICAL_SURFACE('',#9934,0.210000000000001);
#8551=CYLINDRICAL_SURFACE('',#9938,0.210000000000001);
#8552=CYLINDRICAL_SURFACE('',#9942,0.210000000000001);
#8553=CYLINDRICAL_SURFACE('',#9946,0.210000000000001);
#8554=CYLINDRICAL_SURFACE('',#9957,0.21);
#8555=CYLINDRICAL_SURFACE('',#9961,0.21);
#8556=CYLINDRICAL_SURFACE('',#9965,0.21);
#8557=CYLINDRICAL_SURFACE('',#9968,0.21);
#8558=CYLINDRICAL_SURFACE('',#9978,0.21);
#8559=CYLINDRICAL_SURFACE('',#9981,0.21);
#8560=CYLINDRICAL_SURFACE('',#9984,0.21);
#8561=CYLINDRICAL_SURFACE('',#9990,0.21);
#8562=CYLINDRICAL_SURFACE('',#10005,0.625);
#8563=CYLINDRICAL_SURFACE('',#10008,1.5);
#8564=CYLINDRICAL_SURFACE('',#10019,0.21);
#8565=CYLINDRICAL_SURFACE('',#10023,0.21);
#8566=CYLINDRICAL_SURFACE('',#10027,0.21);
#8567=CYLINDRICAL_SURFACE('',#10030,0.21);
#8568=CYLINDRICAL_SURFACE('',#10040,0.21);
#8569=CYLINDRICAL_SURFACE('',#10043,0.21);
#8570=CYLINDRICAL_SURFACE('',#10046,0.21);
#8571=CYLINDRICAL_SURFACE('',#10052,0.21);
#8572=CYLINDRICAL_SURFACE('',#10067,0.625);
#8573=CYLINDRICAL_SURFACE('',#10070,1.5);
#8574=CYLINDRICAL_SURFACE('',#10081,0.21);
#8575=CYLINDRICAL_SURFACE('',#10085,0.21);
#8576=CYLINDRICAL_SURFACE('',#10089,0.21);
#8577=CYLINDRICAL_SURFACE('',#10092,0.21);
#8578=CYLINDRICAL_SURFACE('',#10102,0.21);
#8579=CYLINDRICAL_SURFACE('',#10105,0.21);
#8580=CYLINDRICAL_SURFACE('',#10108,0.21);
#8581=CYLINDRICAL_SURFACE('',#10114,0.21);
#8582=CYLINDRICAL_SURFACE('',#10129,0.625);
#8583=CYLINDRICAL_SURFACE('',#10132,1.5);
#8584=CYLINDRICAL_SURFACE('',#10143,0.21);
#8585=CYLINDRICAL_SURFACE('',#10147,0.21);
#8586=CYLINDRICAL_SURFACE('',#10151,0.21);
#8587=CYLINDRICAL_SURFACE('',#10154,0.21);
#8588=CYLINDRICAL_SURFACE('',#10164,0.21);
#8589=CYLINDRICAL_SURFACE('',#10167,0.21);
#8590=CYLINDRICAL_SURFACE('',#10170,0.21);
#8591=CYLINDRICAL_SURFACE('',#10176,0.21);
#8592=CYLINDRICAL_SURFACE('',#10191,0.625);
#8593=CYLINDRICAL_SURFACE('',#10194,1.5);
#8594=CYLINDRICAL_SURFACE('',#10205,0.21);
#8595=CYLINDRICAL_SURFACE('',#10209,0.21);
#8596=CYLINDRICAL_SURFACE('',#10213,0.21);
#8597=CYLINDRICAL_SURFACE('',#10217,0.21);
#8598=CYLINDRICAL_SURFACE('',#10221,0.6);
#8599=CYLINDRICAL_SURFACE('',#10225,0.8);
#8600=CYLINDRICAL_SURFACE('',#10236,0.275);
#8601=CYLINDRICAL_SURFACE('',#10239,0.275);
#8602=CYLINDRICAL_SURFACE('',#10242,0.275);
#8603=CYLINDRICAL_SURFACE('',#10245,0.275);
#8604=CYLINDRICAL_SURFACE('',#10248,0.275);
#8605=CYLINDRICAL_SURFACE('',#10251,0.275);
#8606=CYLINDRICAL_SURFACE('',#10254,0.275);
#8607=CYLINDRICAL_SURFACE('',#10257,0.275);
#8608=CYLINDRICAL_SURFACE('',#10267,0.51);
#8609=CYLINDRICAL_SURFACE('',#10270,0.8);
#8610=CYLINDRICAL_SURFACE('',#10276,0.21);
#8611=CYLINDRICAL_SURFACE('',#10280,0.5);
#8612=CYLINDRICAL_SURFACE('',#10286,0.5);
#8613=CYLINDRICAL_SURFACE('',#10292,0.21);
#8614=CYLINDRICAL_SURFACE('',#10296,0.5);
#8615=CYLINDRICAL_SURFACE('',#10302,0.5);
#8616=CYLINDRICAL_SURFACE('',#10308,0.21);
#8617=CYLINDRICAL_SURFACE('',#10312,0.5);
#8618=CYLINDRICAL_SURFACE('',#10318,0.5);
#8619=CYLINDRICAL_SURFACE('',#10324,0.21);
#8620=CYLINDRICAL_SURFACE('',#10328,0.5);
#8621=CYLINDRICAL_SURFACE('',#10334,0.5);
#8622=CYLINDRICAL_SURFACE('',#10343,0.6);
#8623=CYLINDRICAL_SURFACE('',#10352,0.525);
#8624=CYLINDRICAL_SURFACE('',#10354,0.525);
#8625=CYLINDRICAL_SURFACE('',#10364,0.225);
#8626=CYLINDRICAL_SURFACE('',#10367,0.165);
#8627=CYLINDRICAL_SURFACE('',#10369,0.275);
#8628=CYLINDRICAL_SURFACE('',#10371,0.275);
#8629=CYLINDRICAL_SURFACE('',#10373,0.6);
#8630=CYLINDRICAL_SURFACE('',#10402,0.425);
#8631=CYLINDRICAL_SURFACE('',#10410,0.24505);
#8632=CYLINDRICAL_SURFACE('',#10416,0.425);
#8633=CYLINDRICAL_SURFACE('',#10424,0.24505);
#8634=CYLINDRICAL_SURFACE('',#10439,0.225);
#8635=CYLINDRICAL_SURFACE('',#10442,0.225);
#8636=CYLINDRICAL_SURFACE('',#10445,0.225);
#8637=CYLINDRICAL_SURFACE('',#10448,0.225);
#8638=CYLINDRICAL_SURFACE('',#10451,0.225);
#8639=CYLINDRICAL_SURFACE('',#10454,0.225);
#8640=CYLINDRICAL_SURFACE('',#10457,0.225);
#8641=CYLINDRICAL_SURFACE('',#10460,0.225);
#8642=CYLINDRICAL_SURFACE('',#10463,0.225);
#8643=CYLINDRICAL_SURFACE('',#10466,0.225);
#8644=CYLINDRICAL_SURFACE('',#10469,0.225);
#8645=CYLINDRICAL_SURFACE('',#10472,0.225);
#8646=CYLINDRICAL_SURFACE('',#10475,0.225);
#8647=CYLINDRICAL_SURFACE('',#10478,0.225);
#8648=CYLINDRICAL_SURFACE('',#10481,0.225);
#8649=CYLINDRICAL_SURFACE('',#10484,0.225);
#8650=CYLINDRICAL_SURFACE('',#10487,0.225);
#8651=CYLINDRICAL_SURFACE('',#10490,0.225);
#8652=CYLINDRICAL_SURFACE('',#10493,0.225);
#8653=CYLINDRICAL_SURFACE('',#10496,0.225);
#8654=CYLINDRICAL_SURFACE('',#10499,0.625);
#8655=CYLINDRICAL_SURFACE('',#10502,0.625);
#8656=CYLINDRICAL_SURFACE('',#10505,0.625);
#8657=CYLINDRICAL_SURFACE('',#10508,0.625);
#8658=CYLINDRICAL_SURFACE('',#10521,0.165);
#8659=CYLINDRICAL_SURFACE('',#10528,0.165);
#8660=CYLINDRICAL_SURFACE('',#10536,0.165);
#8661=CYLINDRICAL_SURFACE('',#10543,0.165);
#8662=CYLINDRICAL_SURFACE('',#10546,1.5);
#8663=CYLINDRICAL_SURFACE('',#10553,1.05);
#8664=CYLINDRICAL_SURFACE('',#10560,2.);
#8665=CYLINDRICAL_SURFACE('',#10562,0.625);
#8666=CYLINDRICAL_SURFACE('',#10570,0.165);
#8667=CYLINDRICAL_SURFACE('',#10577,0.165);
#8668=CYLINDRICAL_SURFACE('',#10585,0.165);
#8669=CYLINDRICAL_SURFACE('',#10592,0.165);
#8670=CYLINDRICAL_SURFACE('',#10595,1.5);
#8671=CYLINDRICAL_SURFACE('',#10602,1.05);
#8672=CYLINDRICAL_SURFACE('',#10609,2.);
#8673=CYLINDRICAL_SURFACE('',#10611,0.625);
#8674=CYLINDRICAL_SURFACE('',#10619,0.165);
#8675=CYLINDRICAL_SURFACE('',#10626,0.165);
#8676=CYLINDRICAL_SURFACE('',#10634,0.165);
#8677=CYLINDRICAL_SURFACE('',#10641,0.165);
#8678=CYLINDRICAL_SURFACE('',#10644,1.5);
#8679=CYLINDRICAL_SURFACE('',#10651,1.05);
#8680=CYLINDRICAL_SURFACE('',#10658,2.);
#8681=CYLINDRICAL_SURFACE('',#10660,0.625);
#8682=CYLINDRICAL_SURFACE('',#10668,0.165);
#8683=CYLINDRICAL_SURFACE('',#10675,0.165);
#8684=CYLINDRICAL_SURFACE('',#10683,0.165);
#8685=CYLINDRICAL_SURFACE('',#10690,0.165);
#8686=CYLINDRICAL_SURFACE('',#10693,1.5);
#8687=CYLINDRICAL_SURFACE('',#10700,1.05);
#8688=CYLINDRICAL_SURFACE('',#10707,2.);
#8689=CYLINDRICAL_SURFACE('',#10709,0.625);
#8690=CYLINDRICAL_SURFACE('',#10714,0.165);
#8691=CYLINDRICAL_SURFACE('',#10717,0.165);
#8692=CYLINDRICAL_SURFACE('',#10720,0.165);
#8693=CYLINDRICAL_SURFACE('',#10723,0.165);
#8694=CYLINDRICAL_SURFACE('',#10729,1.5);
#8695=CYLINDRICAL_SURFACE('',#10731,0.5);
#8696=CYLINDRICAL_SURFACE('',#10747,1.05);
#8697=CYLINDRICAL_SURFACE('',#10751,1.);
#8698=CYLINDRICAL_SURFACE('',#10755,1.05);
#8699=CYLINDRICAL_SURFACE('',#10759,1.);
#8700=CYLINDRICAL_SURFACE('',#10763,1.05);
#8701=CYLINDRICAL_SURFACE('',#10767,0.9);
#8702=CYLINDRICAL_SURFACE('',#10780,0.895);
#8703=CYLINDRICAL_SURFACE('',#10784,0.605);
#8704=CYLINDRICAL_SURFACE('',#10792,0.35);
#8705=CYLINDRICAL_SURFACE('',#10800,0.1954);
#8706=ADVANCED_FACE('',(#1341),#8506,.F.);
#8707=ADVANCED_FACE('',(#1342),#8507,.F.);
#8708=ADVANCED_FACE('',(#1343),#8508,.F.);
#8709=ADVANCED_FACE('',(#1344),#8509,.F.);
#8710=ADVANCED_FACE('',(#1345),#8510,.F.);
#8711=ADVANCED_FACE('',(#1346),#8511,.F.);
#8712=ADVANCED_FACE('',(#1347),#8512,.F.);
#8713=ADVANCED_FACE('',(#1348),#8513,.F.);
#8714=ADVANCED_FACE('',(#1349),#8514,.F.);
#8715=ADVANCED_FACE('',(#1350),#8515,.F.);
#8716=ADVANCED_FACE('',(#1351),#8516,.F.);
#8717=ADVANCED_FACE('',(#1352),#8517,.F.);
#8718=ADVANCED_FACE('',(#1353),#8518,.F.);
#8719=ADVANCED_FACE('',(#1354),#8519,.F.);
#8720=ADVANCED_FACE('',(#1355),#8520,.F.);
#8721=ADVANCED_FACE('',(#1356),#8521,.F.);
#8722=ADVANCED_FACE('',(#1357),#8522,.F.);
#8723=ADVANCED_FACE('',(#1358),#8523,.F.);
#8724=ADVANCED_FACE('',(#1359),#8524,.F.);
#8725=ADVANCED_FACE('',(#1360),#8525,.F.);
#8726=ADVANCED_FACE('',(#1361),#8526,.F.);
#8727=ADVANCED_FACE('',(#1362),#8527,.F.);
#8728=ADVANCED_FACE('',(#1363),#1060,.T.);
#8729=ADVANCED_FACE('',(#1364),#1061,.T.);
#8730=ADVANCED_FACE('',(#1365),#1062,.T.);
#8731=ADVANCED_FACE('',(#1366),#1063,.T.);
#8732=ADVANCED_FACE('',(#1367,#775,#776,#777,#778,#779,#780,#781,#782,#783,
#784,#785,#786,#787,#788,#789,#790,#791,#792,#793,#794,#795,#796),#1064,
 .T.);
#8733=ADVANCED_FACE('',(#1368,#797,#798,#799,#800,#801,#802,#803,#804,#805,
#806,#807,#808,#809,#810,#811,#812,#813,#814,#815,#816,#817,#818),#1065,
 .F.);
#8734=ADVANCED_FACE('',(#1369),#1066,.T.);
#8735=ADVANCED_FACE('',(#1370),#1067,.T.);
#8736=ADVANCED_FACE('',(#1371),#1068,.T.);
#8737=ADVANCED_FACE('',(#1372),#1069,.T.);
#8738=ADVANCED_FACE('',(#1373),#1070,.T.);
#8739=ADVANCED_FACE('',(#1374),#1071,.F.);
#8740=ADVANCED_FACE('',(#1375),#1072,.T.);
#8741=ADVANCED_FACE('',(#1376),#1073,.T.);
#8742=ADVANCED_FACE('',(#1377),#1074,.T.);
#8743=ADVANCED_FACE('',(#1378),#1075,.T.);
#8744=ADVANCED_FACE('',(#1379),#1076,.T.);
#8745=ADVANCED_FACE('',(#1380),#1077,.F.);
#8746=ADVANCED_FACE('',(#1381),#8528,.F.);
#8747=ADVANCED_FACE('',(#1382),#8529,.F.);
#8748=ADVANCED_FACE('',(#1383),#8530,.F.);
#8749=ADVANCED_FACE('',(#1384),#8531,.F.);
#8750=ADVANCED_FACE('',(#1385),#8532,.F.);
#8751=ADVANCED_FACE('',(#1386),#8533,.F.);
#8752=ADVANCED_FACE('',(#1387),#8534,.F.);
#8753=ADVANCED_FACE('',(#1388),#8535,.F.);
#8754=ADVANCED_FACE('',(#1389),#8536,.F.);
#8755=ADVANCED_FACE('',(#1390),#8537,.F.);
#8756=ADVANCED_FACE('',(#1391),#8538,.F.);
#8757=ADVANCED_FACE('',(#1392),#8539,.F.);
#8758=ADVANCED_FACE('',(#1393),#8540,.F.);
#8759=ADVANCED_FACE('',(#1394),#8541,.F.);
#8760=ADVANCED_FACE('',(#1395),#8542,.F.);
#8761=ADVANCED_FACE('',(#1396),#8543,.F.);
#8762=ADVANCED_FACE('',(#1397),#8544,.F.);
#8763=ADVANCED_FACE('',(#1398),#8545,.F.);
#8764=ADVANCED_FACE('',(#1399),#1078,.T.);
#8765=ADVANCED_FACE('',(#1400),#1079,.T.);
#8766=ADVANCED_FACE('',(#1401),#1080,.T.);
#8767=ADVANCED_FACE('',(#1402),#1081,.T.);
#8768=ADVANCED_FACE('',(#1403,#819,#820,#821,#822,#823,#824,#825,#826,#827,
#828,#829,#830,#831,#832,#833,#834,#835,#836),#1082,.T.);
#8769=ADVANCED_FACE('',(#1404,#837,#838,#839,#840,#841,#842,#843,#844,#845,
#846,#847,#848,#849,#850,#851,#852,#853,#854),#1083,.F.);
#8770=ADVANCED_FACE('',(#1405),#8546,.F.);
#8771=ADVANCED_FACE('',(#1406),#1084,.T.);
#8772=ADVANCED_FACE('',(#1407),#8547,.F.);
#8773=ADVANCED_FACE('',(#1408),#1085,.T.);
#8774=ADVANCED_FACE('',(#1409),#8548,.F.);
#8775=ADVANCED_FACE('',(#1410),#1086,.F.);
#8776=ADVANCED_FACE('',(#1411),#8549,.F.);
#8777=ADVANCED_FACE('',(#1412),#1087,.F.);
#8778=ADVANCED_FACE('',(#1413),#1088,.T.);
#8779=ADVANCED_FACE('',(#1414),#1089,.T.);
#8780=ADVANCED_FACE('',(#1415),#1090,.T.);
#8781=ADVANCED_FACE('',(#1416),#1091,.T.);
#8782=ADVANCED_FACE('',(#1417,#855,#856),#1092,.T.);
#8783=ADVANCED_FACE('',(#1418,#857,#858),#1093,.F.);
#8784=ADVANCED_FACE('',(#1419),#8550,.F.);
#8785=ADVANCED_FACE('',(#1420),#1094,.T.);
#8786=ADVANCED_FACE('',(#1421),#8551,.F.);
#8787=ADVANCED_FACE('',(#1422),#1095,.T.);
#8788=ADVANCED_FACE('',(#1423),#8552,.F.);
#8789=ADVANCED_FACE('',(#1424),#1096,.F.);
#8790=ADVANCED_FACE('',(#1425),#8553,.F.);
#8791=ADVANCED_FACE('',(#1426),#1097,.F.);
#8792=ADVANCED_FACE('',(#1427),#1098,.T.);
#8793=ADVANCED_FACE('',(#1428),#1099,.T.);
#8794=ADVANCED_FACE('',(#1429),#1100,.T.);
#8795=ADVANCED_FACE('',(#1430),#1101,.T.);
#8796=ADVANCED_FACE('',(#1431,#859,#860),#1102,.T.);
#8797=ADVANCED_FACE('',(#1432,#861,#862),#1103,.F.);
#8798=ADVANCED_FACE('',(#1433),#8554,.F.);
#8799=ADVANCED_FACE('',(#1434),#1104,.F.);
#8800=ADVANCED_FACE('',(#1435),#8555,.F.);
#8801=ADVANCED_FACE('',(#1436),#1105,.F.);
#8802=ADVANCED_FACE('',(#1437),#8556,.F.);
#8803=ADVANCED_FACE('',(#1438),#8557,.F.);
#8804=ADVANCED_FACE('',(#1439,#863,#864),#1106,.T.);
#8805=ADVANCED_FACE('',(#1440),#1107,.T.);
#8806=ADVANCED_FACE('',(#1441,#865,#866),#1108,.T.);
#8807=ADVANCED_FACE('',(#1442),#1109,.T.);
#8808=ADVANCED_FACE('',(#1443),#1110,.T.);
#8809=ADVANCED_FACE('',(#1444,#867,#868),#1111,.F.);
#8810=ADVANCED_FACE('',(#1445),#8558,.F.);
#8811=ADVANCED_FACE('',(#1446),#8559,.F.);
#8812=ADVANCED_FACE('',(#1447),#8560,.F.);
#8813=ADVANCED_FACE('',(#1448),#1112,.F.);
#8814=ADVANCED_FACE('',(#1449),#8561,.F.);
#8815=ADVANCED_FACE('',(#1450),#1113,.F.);
#8816=ADVANCED_FACE('',(#1451),#1114,.T.);
#8817=ADVANCED_FACE('',(#1452,#869,#870),#1115,.T.);
#8818=ADVANCED_FACE('',(#1453),#1116,.T.);
#8819=ADVANCED_FACE('',(#1454),#1117,.T.);
#8820=ADVANCED_FACE('',(#1455,#871,#872),#1118,.T.);
#8821=ADVANCED_FACE('',(#1456),#1119,.T.);
#8822=ADVANCED_FACE('',(#1457,#873,#874),#1120,.T.);
#8823=ADVANCED_FACE('',(#1458),#1121,.F.);
#8824=ADVANCED_FACE('',(#1459),#8562,.F.);
#8825=ADVANCED_FACE('',(#1460),#8563,.T.);
#8826=ADVANCED_FACE('',(#1461,#875),#1122,.T.);
#8827=ADVANCED_FACE('',(#1462,#876),#1123,.F.);
#8828=ADVANCED_FACE('',(#1463),#590,.T.);
#8829=ADVANCED_FACE('',(#1464),#1124,.T.);
#8830=ADVANCED_FACE('',(#1465),#1125,.F.);
#8831=ADVANCED_FACE('',(#1466),#8564,.F.);
#8832=ADVANCED_FACE('',(#1467),#1126,.F.);
#8833=ADVANCED_FACE('',(#1468),#8565,.F.);
#8834=ADVANCED_FACE('',(#1469),#1127,.F.);
#8835=ADVANCED_FACE('',(#1470),#8566,.F.);
#8836=ADVANCED_FACE('',(#1471),#8567,.F.);
#8837=ADVANCED_FACE('',(#1472,#877,#878),#1128,.T.);
#8838=ADVANCED_FACE('',(#1473),#1129,.T.);
#8839=ADVANCED_FACE('',(#1474,#879,#880),#1130,.T.);
#8840=ADVANCED_FACE('',(#1475),#1131,.T.);
#8841=ADVANCED_FACE('',(#1476),#1132,.T.);
#8842=ADVANCED_FACE('',(#1477,#881,#882),#1133,.F.);
#8843=ADVANCED_FACE('',(#1478),#8568,.F.);
#8844=ADVANCED_FACE('',(#1479),#8569,.F.);
#8845=ADVANCED_FACE('',(#1480),#8570,.F.);
#8846=ADVANCED_FACE('',(#1481),#1134,.F.);
#8847=ADVANCED_FACE('',(#1482),#8571,.F.);
#8848=ADVANCED_FACE('',(#1483),#1135,.F.);
#8849=ADVANCED_FACE('',(#1484),#1136,.T.);
#8850=ADVANCED_FACE('',(#1485,#883,#884),#1137,.T.);
#8851=ADVANCED_FACE('',(#1486),#1138,.T.);
#8852=ADVANCED_FACE('',(#1487),#1139,.T.);
#8853=ADVANCED_FACE('',(#1488,#885,#886),#1140,.T.);
#8854=ADVANCED_FACE('',(#1489),#1141,.T.);
#8855=ADVANCED_FACE('',(#1490,#887,#888),#1142,.T.);
#8856=ADVANCED_FACE('',(#1491),#1143,.F.);
#8857=ADVANCED_FACE('',(#1492),#8572,.F.);
#8858=ADVANCED_FACE('',(#1493),#8573,.T.);
#8859=ADVANCED_FACE('',(#1494,#889),#1144,.T.);
#8860=ADVANCED_FACE('',(#1495,#890),#1145,.F.);
#8861=ADVANCED_FACE('',(#1496),#591,.T.);
#8862=ADVANCED_FACE('',(#1497),#1146,.T.);
#8863=ADVANCED_FACE('',(#1498),#1147,.F.);
#8864=ADVANCED_FACE('',(#1499),#8574,.F.);
#8865=ADVANCED_FACE('',(#1500),#1148,.F.);
#8866=ADVANCED_FACE('',(#1501),#8575,.F.);
#8867=ADVANCED_FACE('',(#1502),#1149,.F.);
#8868=ADVANCED_FACE('',(#1503),#8576,.F.);
#8869=ADVANCED_FACE('',(#1504),#8577,.F.);
#8870=ADVANCED_FACE('',(#1505,#891,#892),#1150,.T.);
#8871=ADVANCED_FACE('',(#1506),#1151,.T.);
#8872=ADVANCED_FACE('',(#1507,#893,#894),#1152,.T.);
#8873=ADVANCED_FACE('',(#1508),#1153,.T.);
#8874=ADVANCED_FACE('',(#1509),#1154,.T.);
#8875=ADVANCED_FACE('',(#1510,#895,#896),#1155,.F.);
#8876=ADVANCED_FACE('',(#1511),#8578,.F.);
#8877=ADVANCED_FACE('',(#1512),#8579,.F.);
#8878=ADVANCED_FACE('',(#1513),#8580,.F.);
#8879=ADVANCED_FACE('',(#1514),#1156,.F.);
#8880=ADVANCED_FACE('',(#1515),#8581,.F.);
#8881=ADVANCED_FACE('',(#1516),#1157,.F.);
#8882=ADVANCED_FACE('',(#1517),#1158,.T.);
#8883=ADVANCED_FACE('',(#1518,#897,#898),#1159,.T.);
#8884=ADVANCED_FACE('',(#1519),#1160,.T.);
#8885=ADVANCED_FACE('',(#1520),#1161,.T.);
#8886=ADVANCED_FACE('',(#1521,#899,#900),#1162,.T.);
#8887=ADVANCED_FACE('',(#1522),#1163,.T.);
#8888=ADVANCED_FACE('',(#1523,#901,#902),#1164,.T.);
#8889=ADVANCED_FACE('',(#1524),#1165,.F.);
#8890=ADVANCED_FACE('',(#1525),#8582,.F.);
#8891=ADVANCED_FACE('',(#1526),#8583,.T.);
#8892=ADVANCED_FACE('',(#1527,#903),#1166,.T.);
#8893=ADVANCED_FACE('',(#1528,#904),#1167,.F.);
#8894=ADVANCED_FACE('',(#1529),#592,.T.);
#8895=ADVANCED_FACE('',(#1530),#1168,.T.);
#8896=ADVANCED_FACE('',(#1531),#1169,.F.);
#8897=ADVANCED_FACE('',(#1532),#8584,.F.);
#8898=ADVANCED_FACE('',(#1533),#1170,.F.);
#8899=ADVANCED_FACE('',(#1534),#8585,.F.);
#8900=ADVANCED_FACE('',(#1535),#1171,.F.);
#8901=ADVANCED_FACE('',(#1536),#8586,.F.);
#8902=ADVANCED_FACE('',(#1537),#8587,.F.);
#8903=ADVANCED_FACE('',(#1538,#905,#906),#1172,.T.);
#8904=ADVANCED_FACE('',(#1539),#1173,.T.);
#8905=ADVANCED_FACE('',(#1540,#907,#908),#1174,.T.);
#8906=ADVANCED_FACE('',(#1541),#1175,.T.);
#8907=ADVANCED_FACE('',(#1542),#1176,.T.);
#8908=ADVANCED_FACE('',(#1543,#909,#910),#1177,.F.);
#8909=ADVANCED_FACE('',(#1544),#8588,.F.);
#8910=ADVANCED_FACE('',(#1545),#8589,.F.);
#8911=ADVANCED_FACE('',(#1546),#8590,.F.);
#8912=ADVANCED_FACE('',(#1547),#1178,.F.);
#8913=ADVANCED_FACE('',(#1548),#8591,.F.);
#8914=ADVANCED_FACE('',(#1549),#1179,.F.);
#8915=ADVANCED_FACE('',(#1550),#1180,.T.);
#8916=ADVANCED_FACE('',(#1551,#911,#912),#1181,.T.);
#8917=ADVANCED_FACE('',(#1552),#1182,.T.);
#8918=ADVANCED_FACE('',(#1553),#1183,.T.);
#8919=ADVANCED_FACE('',(#1554,#913,#914),#1184,.T.);
#8920=ADVANCED_FACE('',(#1555),#1185,.T.);
#8921=ADVANCED_FACE('',(#1556,#915,#916),#1186,.T.);
#8922=ADVANCED_FACE('',(#1557),#1187,.F.);
#8923=ADVANCED_FACE('',(#1558),#8592,.F.);
#8924=ADVANCED_FACE('',(#1559),#8593,.T.);
#8925=ADVANCED_FACE('',(#1560,#917),#1188,.T.);
#8926=ADVANCED_FACE('',(#1561,#918),#1189,.F.);
#8927=ADVANCED_FACE('',(#1562),#593,.T.);
#8928=ADVANCED_FACE('',(#1563),#1190,.T.);
#8929=ADVANCED_FACE('',(#1564),#1191,.F.);
#8930=ADVANCED_FACE('',(#1565),#8594,.F.);
#8931=ADVANCED_FACE('',(#1566),#1192,.F.);
#8932=ADVANCED_FACE('',(#1567),#8595,.F.);
#8933=ADVANCED_FACE('',(#1568),#1193,.F.);
#8934=ADVANCED_FACE('',(#1569),#8596,.F.);
#8935=ADVANCED_FACE('',(#1570),#1194,.F.);
#8936=ADVANCED_FACE('',(#1571),#8597,.F.);
#8937=ADVANCED_FACE('',(#1572),#1195,.F.);
#8938=ADVANCED_FACE('',(#1573),#8598,.F.);
#8939=ADVANCED_FACE('',(#1574),#1196,.T.);
#8940=ADVANCED_FACE('',(#1575),#8599,.F.);
#8941=ADVANCED_FACE('',(#1576,#919),#1197,.T.);
#8942=ADVANCED_FACE('',(#1577),#1198,.T.);
#8943=ADVANCED_FACE('',(#1578),#1199,.T.);
#8944=ADVANCED_FACE('',(#1579),#1200,.T.);
#8945=ADVANCED_FACE('',(#1580),#1201,.T.);
#8946=ADVANCED_FACE('',(#1581,#920),#1202,.T.);
#8947=ADVANCED_FACE('',(#1582,#921,#922,#923,#924),#1203,.F.);
#8948=ADVANCED_FACE('',(#1583),#8600,.F.);
#8949=ADVANCED_FACE('',(#1584),#8601,.F.);
#8950=ADVANCED_FACE('',(#1585),#8602,.F.);
#8951=ADVANCED_FACE('',(#1586),#8603,.F.);
#8952=ADVANCED_FACE('',(#1587),#8604,.F.);
#8953=ADVANCED_FACE('',(#1588),#8605,.F.);
#8954=ADVANCED_FACE('',(#1589),#8606,.F.);
#8955=ADVANCED_FACE('',(#1590),#8607,.F.);
#8956=ADVANCED_FACE('',(#1591),#1204,.T.);
#8957=ADVANCED_FACE('',(#1592),#1205,.T.);
#8958=ADVANCED_FACE('',(#1593),#1206,.T.);
#8959=ADVANCED_FACE('',(#1594),#1207,.T.);
#8960=ADVANCED_FACE('',(#1595,#925,#926,#927,#928,#929,#930,#931,#932),
#1208,.T.);
#8961=ADVANCED_FACE('',(#1596,#933,#934,#935,#936,#937,#938,#939,#940),
#1209,.F.);
#8962=ADVANCED_FACE('',(#1597),#8608,.F.);
#8963=ADVANCED_FACE('',(#1598),#8609,.T.);
#8964=ADVANCED_FACE('',(#1599,#941),#1210,.T.);
#8965=ADVANCED_FACE('',(#1600,#942),#1211,.F.);
#8966=ADVANCED_FACE('',(#1601),#8610,.F.);
#8967=ADVANCED_FACE('',(#1602),#1212,.F.);
#8968=ADVANCED_FACE('',(#1603),#8611,.T.);
#8969=ADVANCED_FACE('',(#1604),#1213,.T.);
#8970=ADVANCED_FACE('',(#1605,#943),#1214,.F.);
#8971=ADVANCED_FACE('',(#1606),#8612,.T.);
#8972=ADVANCED_FACE('',(#1607),#1215,.T.);
#8973=ADVANCED_FACE('',(#1608),#1216,.F.);
#8974=ADVANCED_FACE('',(#1609),#8613,.F.);
#8975=ADVANCED_FACE('',(#1610),#1217,.T.);
#8976=ADVANCED_FACE('',(#1611),#8614,.T.);
#8977=ADVANCED_FACE('',(#1612,#944),#1218,.T.);
#8978=ADVANCED_FACE('',(#1613),#1219,.F.);
#8979=ADVANCED_FACE('',(#1614),#8615,.T.);
#8980=ADVANCED_FACE('',(#1615),#1220,.T.);
#8981=ADVANCED_FACE('',(#1616),#1221,.F.);
#8982=ADVANCED_FACE('',(#1617),#8616,.F.);
#8983=ADVANCED_FACE('',(#1618),#1222,.F.);
#8984=ADVANCED_FACE('',(#1619),#8617,.T.);
#8985=ADVANCED_FACE('',(#1620),#1223,.T.);
#8986=ADVANCED_FACE('',(#1621,#945),#1224,.F.);
#8987=ADVANCED_FACE('',(#1622),#8618,.T.);
#8988=ADVANCED_FACE('',(#1623),#1225,.T.);
#8989=ADVANCED_FACE('',(#1624),#1226,.F.);
#8990=ADVANCED_FACE('',(#1625),#8619,.F.);
#8991=ADVANCED_FACE('',(#1626),#1227,.T.);
#8992=ADVANCED_FACE('',(#1627),#8620,.T.);
#8993=ADVANCED_FACE('',(#1628,#946),#1228,.T.);
#8994=ADVANCED_FACE('',(#1629),#1229,.F.);
#8995=ADVANCED_FACE('',(#1630),#8621,.T.);
#8996=ADVANCED_FACE('',(#1631),#1230,.T.);
#8997=ADVANCED_FACE('',(#1632),#1231,.F.);
#8998=ADVANCED_FACE('',(#1633),#573,.T.);
#8999=ADVANCED_FACE('',(#1634),#8622,.T.);
#9000=ADVANCED_FACE('',(#1635),#1232,.F.);
#9001=ADVANCED_FACE('',(#1636),#574,.T.);
#9002=ADVANCED_FACE('',(#1637),#1233,.T.);
#9003=ADVANCED_FACE('',(#1638),#1234,.F.);
#9004=ADVANCED_FACE('',(#1639),#8623,.F.);
#9005=ADVANCED_FACE('',(#1640),#8624,.F.);
#9006=ADVANCED_FACE('',(#1641),#1235,.F.);
#9007=ADVANCED_FACE('',(#1642,#947),#1236,.T.);
#9008=ADVANCED_FACE('',(#1643,#948),#1237,.T.);
#9009=ADVANCED_FACE('',(#1644,#949),#1238,.T.);
#9010=ADVANCED_FACE('',(#1645),#8625,.F.);
#9011=ADVANCED_FACE('',(#1646),#8626,.F.);
#9012=ADVANCED_FACE('',(#1647),#8627,.F.);
#9013=ADVANCED_FACE('',(#1648),#8628,.F.);
#9014=ADVANCED_FACE('',(#1649),#8629,.F.);
#9015=ADVANCED_FACE('',(#1650,#950),#1239,.T.);
#9016=ADVANCED_FACE('',(#1651),#1240,.T.);
#9017=ADVANCED_FACE('',(#1652,#951,#952),#1241,.T.);
#9018=ADVANCED_FACE('',(#1653),#1242,.T.);
#9019=ADVANCED_FACE('',(#1654,#953),#1243,.T.);
#9020=ADVANCED_FACE('',(#1655),#1244,.T.);
#9021=ADVANCED_FACE('',(#1656,#954),#1245,.T.);
#9022=ADVANCED_FACE('',(#1657),#1246,.T.);
#9023=ADVANCED_FACE('',(#1658,#955),#1247,.T.);
#9024=ADVANCED_FACE('',(#1659),#1248,.T.);
#9025=ADVANCED_FACE('',(#1660,#956),#1249,.T.);
#9026=ADVANCED_FACE('',(#1661),#1250,.F.);
#9027=ADVANCED_FACE('',(#1662),#1251,.F.);
#9028=ADVANCED_FACE('',(#1663),#1252,.F.);
#9029=ADVANCED_FACE('',(#1664),#1253,.F.);
#9030=ADVANCED_FACE('',(#1665),#1254,.F.);
#9031=ADVANCED_FACE('',(#1666),#1255,.F.);
#9032=ADVANCED_FACE('',(#1667),#1256,.F.);
#9033=ADVANCED_FACE('',(#1668),#1257,.F.);
#9034=ADVANCED_FACE('',(#1669),#1258,.F.);
#9035=ADVANCED_FACE('',(#1670),#1259,.T.);
#9036=ADVANCED_FACE('',(#1671),#575,.T.);
#9037=ADVANCED_FACE('',(#1672),#8630,.T.);
#9038=ADVANCED_FACE('',(#1673),#576,.T.);
#9039=ADVANCED_FACE('',(#1674,#957),#1260,.T.);
#9040=ADVANCED_FACE('',(#1675),#577,.T.);
#9041=ADVANCED_FACE('',(#1676),#8631,.T.);
#9042=ADVANCED_FACE('',(#1677),#1261,.T.);
#9043=ADVANCED_FACE('',(#1678),#578,.T.);
#9044=ADVANCED_FACE('',(#1679),#8632,.T.);
#9045=ADVANCED_FACE('',(#1680),#579,.T.);
#9046=ADVANCED_FACE('',(#1681,#958),#1262,.T.);
#9047=ADVANCED_FACE('',(#1682),#580,.T.);
#9048=ADVANCED_FACE('',(#1683),#8633,.T.);
#9049=ADVANCED_FACE('',(#1684),#581,.T.);
#9050=ADVANCED_FACE('',(#1685),#1263,.T.);
#9051=ADVANCED_FACE('',(#1686),#1264,.F.);
#9052=ADVANCED_FACE('',(#1687),#1265,.F.);
#9053=ADVANCED_FACE('',(#1688),#1266,.F.);
#9054=ADVANCED_FACE('',(#1689),#1267,.F.);
#9055=ADVANCED_FACE('',(#1690),#1268,.F.);
#9056=ADVANCED_FACE('',(#1691),#1269,.F.);
#9057=ADVANCED_FACE('',(#1692),#1270,.F.);
#9058=ADVANCED_FACE('',(#1693),#1271,.F.);
#9059=ADVANCED_FACE('',(#1694),#8634,.F.);
#9060=ADVANCED_FACE('',(#1695),#8635,.F.);
#9061=ADVANCED_FACE('',(#1696),#8636,.F.);
#9062=ADVANCED_FACE('',(#1697),#8637,.F.);
#9063=ADVANCED_FACE('',(#1698),#8638,.F.);
#9064=ADVANCED_FACE('',(#1699),#8639,.F.);
#9065=ADVANCED_FACE('',(#1700),#8640,.F.);
#9066=ADVANCED_FACE('',(#1701),#8641,.F.);
#9067=ADVANCED_FACE('',(#1702),#8642,.F.);
#9068=ADVANCED_FACE('',(#1703),#8643,.F.);
#9069=ADVANCED_FACE('',(#1704),#8644,.F.);
#9070=ADVANCED_FACE('',(#1705),#8645,.F.);
#9071=ADVANCED_FACE('',(#1706),#8646,.F.);
#9072=ADVANCED_FACE('',(#1707),#8647,.F.);
#9073=ADVANCED_FACE('',(#1708),#8648,.F.);
#9074=ADVANCED_FACE('',(#1709),#8649,.F.);
#9075=ADVANCED_FACE('',(#1710),#8650,.F.);
#9076=ADVANCED_FACE('',(#1711),#8651,.F.);
#9077=ADVANCED_FACE('',(#1712),#8652,.F.);
#9078=ADVANCED_FACE('',(#1713),#8653,.F.);
#9079=ADVANCED_FACE('',(#1714),#8654,.F.);
#9080=ADVANCED_FACE('',(#1715),#8655,.F.);
#9081=ADVANCED_FACE('',(#1716),#8656,.F.);
#9082=ADVANCED_FACE('',(#1717),#8657,.F.);
#9083=ADVANCED_FACE('',(#1718),#1272,.T.);
#9084=ADVANCED_FACE('',(#1719),#1273,.T.);
#9085=ADVANCED_FACE('',(#1720),#1274,.T.);
#9086=ADVANCED_FACE('',(#1721),#1275,.T.);
#9087=ADVANCED_FACE('',(#1722,#959,#960,#961,#962,#963,#964,#965,#966,#967,
#968,#969,#970,#971,#972,#973,#974,#975,#976,#977,#978,#979,#980,#981,#982),
#1276,.T.);
#9088=ADVANCED_FACE('',(#1723,#983,#984,#985,#986,#987,#988,#989,#990,#991,
#992,#993,#994,#995,#996,#997,#998,#999,#1000,#1001,#1002,#1003,#1004,#1005,
#1006),#1277,.F.);
#9089=ADVANCED_FACE('',(#1724),#1278,.T.);
#9090=ADVANCED_FACE('',(#1725),#8658,.F.);
#9091=ADVANCED_FACE('',(#1726),#1279,.T.);
#9092=ADVANCED_FACE('',(#1727),#8659,.F.);
#9093=ADVANCED_FACE('',(#1728),#1280,.T.);
#9094=ADVANCED_FACE('',(#1729),#8660,.F.);
#9095=ADVANCED_FACE('',(#1730),#1281,.T.);
#9096=ADVANCED_FACE('',(#1731),#8661,.F.);
#9097=ADVANCED_FACE('',(#1732),#8662,.T.);
#9098=ADVANCED_FACE('',(#1733),#8663,.F.);
#9099=ADVANCED_FACE('',(#1734,#1007),#1282,.T.);
#9100=ADVANCED_FACE('',(#1735,#1008),#1283,.F.);
#9101=ADVANCED_FACE('',(#1736),#8664,.T.);
#9102=ADVANCED_FACE('',(#1737),#8665,.F.);
#9103=ADVANCED_FACE('',(#1738,#1009,#1010,#1011,#1012,#1013),#1284,.T.);
#9104=ADVANCED_FACE('',(#1739,#1014),#1285,.F.);
#9105=ADVANCED_FACE('',(#1740),#1286,.T.);
#9106=ADVANCED_FACE('',(#1741),#8666,.F.);
#9107=ADVANCED_FACE('',(#1742),#1287,.T.);
#9108=ADVANCED_FACE('',(#1743),#8667,.F.);
#9109=ADVANCED_FACE('',(#1744),#1288,.T.);
#9110=ADVANCED_FACE('',(#1745),#8668,.F.);
#9111=ADVANCED_FACE('',(#1746),#1289,.T.);
#9112=ADVANCED_FACE('',(#1747),#8669,.F.);
#9113=ADVANCED_FACE('',(#1748),#8670,.T.);
#9114=ADVANCED_FACE('',(#1749),#8671,.F.);
#9115=ADVANCED_FACE('',(#1750,#1015),#1290,.T.);
#9116=ADVANCED_FACE('',(#1751,#1016),#1291,.F.);
#9117=ADVANCED_FACE('',(#1752),#8672,.T.);
#9118=ADVANCED_FACE('',(#1753),#8673,.F.);
#9119=ADVANCED_FACE('',(#1754,#1017,#1018,#1019,#1020,#1021),#1292,.T.);
#9120=ADVANCED_FACE('',(#1755,#1022),#1293,.F.);
#9121=ADVANCED_FACE('',(#1756),#1294,.T.);
#9122=ADVANCED_FACE('',(#1757),#8674,.F.);
#9123=ADVANCED_FACE('',(#1758),#1295,.T.);
#9124=ADVANCED_FACE('',(#1759),#8675,.F.);
#9125=ADVANCED_FACE('',(#1760),#1296,.T.);
#9126=ADVANCED_FACE('',(#1761),#8676,.F.);
#9127=ADVANCED_FACE('',(#1762),#1297,.T.);
#9128=ADVANCED_FACE('',(#1763),#8677,.F.);
#9129=ADVANCED_FACE('',(#1764),#8678,.T.);
#9130=ADVANCED_FACE('',(#1765),#8679,.F.);
#9131=ADVANCED_FACE('',(#1766,#1023),#1298,.T.);
#9132=ADVANCED_FACE('',(#1767,#1024),#1299,.F.);
#9133=ADVANCED_FACE('',(#1768),#8680,.T.);
#9134=ADVANCED_FACE('',(#1769),#8681,.F.);
#9135=ADVANCED_FACE('',(#1770,#1025,#1026,#1027,#1028,#1029),#1300,.T.);
#9136=ADVANCED_FACE('',(#1771,#1030),#1301,.F.);
#9137=ADVANCED_FACE('',(#1772),#1302,.T.);
#9138=ADVANCED_FACE('',(#1773),#8682,.F.);
#9139=ADVANCED_FACE('',(#1774),#1303,.T.);
#9140=ADVANCED_FACE('',(#1775),#8683,.F.);
#9141=ADVANCED_FACE('',(#1776),#1304,.T.);
#9142=ADVANCED_FACE('',(#1777),#8684,.F.);
#9143=ADVANCED_FACE('',(#1778),#1305,.T.);
#9144=ADVANCED_FACE('',(#1779),#8685,.F.);
#9145=ADVANCED_FACE('',(#1780),#8686,.T.);
#9146=ADVANCED_FACE('',(#1781),#8687,.F.);
#9147=ADVANCED_FACE('',(#1782,#1031),#1306,.T.);
#9148=ADVANCED_FACE('',(#1783,#1032),#1307,.F.);
#9149=ADVANCED_FACE('',(#1784),#8688,.T.);
#9150=ADVANCED_FACE('',(#1785),#8689,.F.);
#9151=ADVANCED_FACE('',(#1786,#1033,#1034,#1035,#1036,#1037),#1308,.T.);
#9152=ADVANCED_FACE('',(#1787,#1038),#1309,.F.);
#9153=ADVANCED_FACE('',(#1788),#8690,.F.);
#9154=ADVANCED_FACE('',(#1789),#8691,.F.);
#9155=ADVANCED_FACE('',(#1790),#8692,.F.);
#9156=ADVANCED_FACE('',(#1791),#8693,.F.);
#9157=ADVANCED_FACE('',(#1792,#1039,#1040,#1041,#1042,#1043),#1310,.F.);
#9158=ADVANCED_FACE('',(#1793),#8694,.T.);
#9159=ADVANCED_FACE('',(#1794),#8695,.T.);
#9160=ADVANCED_FACE('',(#1795,#1044,#1045,#1046,#1047),#1311,.T.);
#9161=ADVANCED_FACE('',(#1796),#1312,.F.);
#9162=ADVANCED_FACE('',(#1797),#1313,.F.);
#9163=ADVANCED_FACE('',(#1798),#1314,.F.);
#9164=ADVANCED_FACE('',(#1799),#1315,.F.);
#9165=ADVANCED_FACE('',(#1800),#1316,.F.);
#9166=ADVANCED_FACE('',(#1801),#1317,.F.);
#9167=ADVANCED_FACE('',(#1802,#1048),#1318,.T.);
#9168=ADVANCED_FACE('',(#1803),#8696,.T.);
#9169=ADVANCED_FACE('',(#1804,#1049),#1319,.T.);
#9170=ADVANCED_FACE('',(#1805),#8697,.T.);
#9171=ADVANCED_FACE('',(#1806,#1050),#1320,.T.);
#9172=ADVANCED_FACE('',(#1807),#8698,.T.);
#9173=ADVANCED_FACE('',(#1808,#1051),#1321,.T.);
#9174=ADVANCED_FACE('',(#1809),#8699,.T.);
#9175=ADVANCED_FACE('',(#1810,#1052),#1322,.T.);
#9176=ADVANCED_FACE('',(#1811),#8700,.T.);
#9177=ADVANCED_FACE('',(#1812,#1053),#1323,.T.);
#9178=ADVANCED_FACE('',(#1813,#1054),#8701,.F.);
#9179=ADVANCED_FACE('',(#1814),#1324,.F.);
#9180=ADVANCED_FACE('',(#1815),#1325,.F.);
#9181=ADVANCED_FACE('',(#1816),#1326,.F.);
#9182=ADVANCED_FACE('',(#1817),#1327,.F.);
#9183=ADVANCED_FACE('',(#1818,#1055),#1328,.T.);
#9184=ADVANCED_FACE('',(#1819,#1056),#8702,.T.);
#9185=ADVANCED_FACE('',(#1820,#1057),#1329,.T.);
#9186=ADVANCED_FACE('',(#1821,#1058),#8703,.F.);
#9187=ADVANCED_FACE('',(#1822),#1330,.T.);
#9188=ADVANCED_FACE('',(#1823),#582,.T.);
#9189=ADVANCED_FACE('',(#1824),#8704,.T.);
#9190=ADVANCED_FACE('',(#1825),#583,.T.);
#9191=ADVANCED_FACE('',(#1826,#1059),#1331,.T.);
#9192=ADVANCED_FACE('',(#1827),#584,.T.);
#9193=ADVANCED_FACE('',(#1828),#8705,.T.);
#9194=ADVANCED_FACE('',(#1829),#585,.T.);
#9195=ADVANCED_FACE('',(#1830),#1332,.T.);
#9196=ADVANCED_FACE('',(#1831),#1333,.F.);
#9197=ADVANCED_FACE('',(#1832),#1334,.F.);
#9198=ADVANCED_FACE('',(#1833),#1335,.F.);
#9199=ADVANCED_FACE('',(#1834),#1336,.F.);
#9200=ADVANCED_FACE('',(#1835),#1337,.F.);
#9201=ADVANCED_FACE('',(#1836),#1338,.F.);
#9202=ADVANCED_FACE('',(#1837),#1339,.F.);
#9203=ADVANCED_FACE('',(#1838),#1340,.F.);
#9204=CLOSED_SHELL('',(#8706,#8707,#8708,#8709,#8710,#8711,#8712,#8713,
#8714,#8715,#8716,#8717,#8718,#8719,#8720,#8721,#8722,#8723,#8724,#8725,
#8726,#8727,#8728,#8729,#8730,#8731,#8732,#8733));
#9205=CLOSED_SHELL('',(#8734,#8735,#8736,#8737,#8738,#8739));
#9206=CLOSED_SHELL('',(#8740,#8741,#8742,#8743,#8744,#8745));
#9207=CLOSED_SHELL('',(#8746,#8747,#8748,#8749,#8750,#8751,#8752,#8753,
#8754,#8755,#8756,#8757,#8758,#8759,#8760,#8761,#8762,#8763,#8764,#8765,
#8766,#8767,#8768,#8769));
#9208=CLOSED_SHELL('',(#8770,#8771,#8772,#8773,#8774,#8775,#8776,#8777,
#8778,#8779,#8780,#8781,#8782,#8783));
#9209=CLOSED_SHELL('',(#8784,#8785,#8786,#8787,#8788,#8789,#8790,#8791,
#8792,#8793,#8794,#8795,#8796,#8797));
#9210=CLOSED_SHELL('',(#8798,#8799,#8800,#8801,#8802,#8803,#8804,#8805,
#8806,#8807,#8808,#8809));
#9211=CLOSED_SHELL('',(#8810,#8811,#8812,#8813,#8814,#8815,#8816,#8817,
#8818,#8819,#8820,#8821,#8822,#8823));
#9212=CLOSED_SHELL('',(#8824,#8825,#8826,#8827));
#9213=CLOSED_SHELL('',(#8828,#8829,#8830));
#9214=CLOSED_SHELL('',(#8831,#8832,#8833,#8834,#8835,#8836,#8837,#8838,
#8839,#8840,#8841,#8842));
#9215=CLOSED_SHELL('',(#8843,#8844,#8845,#8846,#8847,#8848,#8849,#8850,
#8851,#8852,#8853,#8854,#8855,#8856));
#9216=CLOSED_SHELL('',(#8857,#8858,#8859,#8860));
#9217=CLOSED_SHELL('',(#8861,#8862,#8863));
#9218=CLOSED_SHELL('',(#8864,#8865,#8866,#8867,#8868,#8869,#8870,#8871,
#8872,#8873,#8874,#8875));
#9219=CLOSED_SHELL('',(#8876,#8877,#8878,#8879,#8880,#8881,#8882,#8883,
#8884,#8885,#8886,#8887,#8888,#8889));
#9220=CLOSED_SHELL('',(#8890,#8891,#8892,#8893));
#9221=CLOSED_SHELL('',(#8894,#8895,#8896));
#9222=CLOSED_SHELL('',(#8897,#8898,#8899,#8900,#8901,#8902,#8903,#8904,
#8905,#8906,#8907,#8908));
#9223=CLOSED_SHELL('',(#8909,#8910,#8911,#8912,#8913,#8914,#8915,#8916,
#8917,#8918,#8919,#8920,#8921,#8922));
#9224=CLOSED_SHELL('',(#8923,#8924,#8925,#8926));
#9225=CLOSED_SHELL('',(#8927,#8928,#8929));
#9226=CLOSED_SHELL('',(#8930,#8931,#8932,#8933,#8934,#8935,#8936,#8937,
#8938,#8939,#8940,#8941,#8942,#8943,#8944,#8945,#8946,#8947));
#9227=CLOSED_SHELL('',(#8948,#8949,#8950,#8951,#8952,#8953,#8954,#8955,
#8956,#8957,#8958,#8959,#8960,#8961));
#9228=CLOSED_SHELL('',(#8962,#8963,#8964,#8965));
#9229=CLOSED_SHELL('',(#8966,#8967,#8968,#8969,#8970));
#9230=CLOSED_SHELL('',(#8971,#8972,#8973));
#9231=CLOSED_SHELL('',(#8974,#8975,#8976,#8977,#8978));
#9232=CLOSED_SHELL('',(#8979,#8980,#8981));
#9233=CLOSED_SHELL('',(#8982,#8983,#8984,#8985,#8986));
#9234=CLOSED_SHELL('',(#8987,#8988,#8989));
#9235=CLOSED_SHELL('',(#8990,#8991,#8992,#8993,#8994));
#9236=CLOSED_SHELL('',(#8995,#8996,#8997));
#9237=CLOSED_SHELL('',(#8998,#8999,#9000,#9001,#9002));
#9238=CLOSED_SHELL('',(#9003,#9004,#9005,#9006,#9007,#9008,#9009,#9010,
#9011,#9012,#9013,#9014,#9015,#9016,#9017,#9018,#9019,#9020,#9021,#9022,
#9023,#9024,#9025));
#9239=CLOSED_SHELL('',(#9026,#9027,#9028,#9029,#9030,#9031,#9032,#9033));
#9240=CLOSED_SHELL('',(#9034,#9035,#9036,#9037,#9038,#9039,#9040,#9041));
#9241=CLOSED_SHELL('',(#9042,#9043,#9044,#9045,#9046,#9047,#9048,#9049,
#9050));
#9242=CLOSED_SHELL('',(#9051,#9052,#9053,#9054,#9055,#9056,#9057,#9058));
#9243=CLOSED_SHELL('',(#9059,#9060,#9061,#9062,#9063,#9064,#9065,#9066,
#9067,#9068,#9069,#9070,#9071,#9072,#9073,#9074,#9075,#9076,#9077,#9078,
#9079,#9080,#9081,#9082,#9083,#9084,#9085,#9086,#9087,#9088));
#9244=CLOSED_SHELL('',(#9089,#9090,#9091,#9092,#9093,#9094,#9095,#9096,
#9097,#9098,#9099,#9100,#9101,#9102,#9103,#9104));
#9245=CLOSED_SHELL('',(#9105,#9106,#9107,#9108,#9109,#9110,#9111,#9112,
#9113,#9114,#9115,#9116,#9117,#9118,#9119,#9120));
#9246=CLOSED_SHELL('',(#9121,#9122,#9123,#9124,#9125,#9126,#9127,#9128,
#9129,#9130,#9131,#9132,#9133,#9134,#9135,#9136));
#9247=CLOSED_SHELL('',(#9137,#9138,#9139,#9140,#9141,#9142,#9143,#9144,
#9145,#9146,#9147,#9148,#9149,#9150,#9151,#9152));
#9248=CLOSED_SHELL('',(#9153,#9154,#9155,#9156,#9157,#9158,#9159,#9160,
#9161));
#9249=CLOSED_SHELL('',(#9162,#9163,#9164,#9165,#9166,#9167,#9168,#9169,
#9170,#9171,#9172,#9173,#9174,#9175,#9176,#9177,#9178));
#9250=CLOSED_SHELL('',(#9179,#9180,#9181,#9182,#9183,#9184,#9185,#9186));
#9251=CLOSED_SHELL('',(#9187,#9188,#9189,#9190,#9191,#9192,#9193,#9194,
#9195));
#9252=CLOSED_SHELL('',(#9196,#9197,#9198,#9199,#9200,#9201,#9202,#9203));
#9253=DERIVED_UNIT_ELEMENT(#9345,1.);
#9254=DERIVED_UNIT_ELEMENT(#22396,-3.);
#9255=DERIVED_UNIT_ELEMENT(#9345,1.);
#9256=DERIVED_UNIT_ELEMENT(#22396,-3.);
#9257=DERIVED_UNIT_ELEMENT(#9345,1.);
#9258=DERIVED_UNIT_ELEMENT(#22396,-3.);
#9259=DERIVED_UNIT_ELEMENT(#9345,1.);
#9260=DERIVED_UNIT_ELEMENT(#22396,-3.);
#9261=DERIVED_UNIT_ELEMENT(#9345,1.);
#9262=DERIVED_UNIT_ELEMENT(#22396,-3.);
#9263=DERIVED_UNIT_ELEMENT(#9345,1.);
#9264=DERIVED_UNIT_ELEMENT(#22396,-3.);
#9265=DERIVED_UNIT_ELEMENT(#9345,1.);
#9266=DERIVED_UNIT_ELEMENT(#22396,-3.);
#9267=DERIVED_UNIT_ELEMENT(#9345,1.);
#9268=DERIVED_UNIT_ELEMENT(#22396,-3.);
#9269=DERIVED_UNIT_ELEMENT(#9345,1.);
#9270=DERIVED_UNIT_ELEMENT(#22396,-3.);
#9271=DERIVED_UNIT_ELEMENT(#9345,1.);
#9272=DERIVED_UNIT_ELEMENT(#22396,-3.);
#9273=DERIVED_UNIT_ELEMENT(#9345,1.);
#9274=DERIVED_UNIT_ELEMENT(#22396,-3.);
#9275=DERIVED_UNIT_ELEMENT(#9345,1.);
#9276=DERIVED_UNIT_ELEMENT(#22396,-3.);
#9277=DERIVED_UNIT_ELEMENT(#9345,1.);
#9278=DERIVED_UNIT_ELEMENT(#22396,-3.);
#9279=DERIVED_UNIT_ELEMENT(#9345,1.);
#9280=DERIVED_UNIT_ELEMENT(#22396,-3.);
#9281=DERIVED_UNIT_ELEMENT(#9345,1.);
#9282=DERIVED_UNIT_ELEMENT(#22396,-3.);
#9283=DERIVED_UNIT_ELEMENT(#9345,1.);
#9284=DERIVED_UNIT_ELEMENT(#22396,-3.);
#9285=DERIVED_UNIT_ELEMENT(#9345,1.);
#9286=DERIVED_UNIT_ELEMENT(#22396,-3.);
#9287=DERIVED_UNIT_ELEMENT(#9345,1.);
#9288=DERIVED_UNIT_ELEMENT(#22396,-3.);
#9289=DERIVED_UNIT_ELEMENT(#9345,1.);
#9290=DERIVED_UNIT_ELEMENT(#22396,-3.);
#9291=DERIVED_UNIT_ELEMENT(#9345,1.);
#9292=DERIVED_UNIT_ELEMENT(#22396,-3.);
#9293=DERIVED_UNIT_ELEMENT(#9345,1.);
#9294=DERIVED_UNIT_ELEMENT(#22396,-3.);
#9295=DERIVED_UNIT_ELEMENT(#9345,1.);
#9296=DERIVED_UNIT_ELEMENT(#22396,-3.);
#9297=DERIVED_UNIT_ELEMENT(#9345,1.);
#9298=DERIVED_UNIT_ELEMENT(#22396,-3.);
#9299=DERIVED_UNIT_ELEMENT(#9345,1.);
#9300=DERIVED_UNIT_ELEMENT(#22396,-3.);
#9301=DERIVED_UNIT_ELEMENT(#9345,1.);
#9302=DERIVED_UNIT_ELEMENT(#22396,-3.);
#9303=DERIVED_UNIT_ELEMENT(#9345,1.);
#9304=DERIVED_UNIT_ELEMENT(#22396,-3.);
#9305=DERIVED_UNIT_ELEMENT(#9345,1.);
#9306=DERIVED_UNIT_ELEMENT(#22396,-3.);
#9307=DERIVED_UNIT_ELEMENT(#9345,1.);
#9308=DERIVED_UNIT_ELEMENT(#22396,-3.);
#9309=DERIVED_UNIT_ELEMENT(#9345,1.);
#9310=DERIVED_UNIT_ELEMENT(#22396,-3.);
#9311=DERIVED_UNIT_ELEMENT(#9345,1.);
#9312=DERIVED_UNIT_ELEMENT(#22396,-3.);
#9313=DERIVED_UNIT_ELEMENT(#9345,1.);
#9314=DERIVED_UNIT_ELEMENT(#22396,-3.);
#9315=DERIVED_UNIT_ELEMENT(#9345,1.);
#9316=DERIVED_UNIT_ELEMENT(#22396,-3.);
#9317=DERIVED_UNIT_ELEMENT(#9345,1.);
#9318=DERIVED_UNIT_ELEMENT(#22396,-3.);
#9319=DERIVED_UNIT_ELEMENT(#9345,1.);
#9320=DERIVED_UNIT_ELEMENT(#22396,-3.);
#9321=DERIVED_UNIT_ELEMENT(#9345,1.);
#9322=DERIVED_UNIT_ELEMENT(#22396,-3.);
#9323=DERIVED_UNIT_ELEMENT(#9345,1.);
#9324=DERIVED_UNIT_ELEMENT(#22396,-3.);
#9325=DERIVED_UNIT_ELEMENT(#9345,1.);
#9326=DERIVED_UNIT_ELEMENT(#22396,-3.);
#9327=DERIVED_UNIT_ELEMENT(#9345,1.);
#9328=DERIVED_UNIT_ELEMENT(#22396,-3.);
#9329=DERIVED_UNIT_ELEMENT(#9345,1.);
#9330=DERIVED_UNIT_ELEMENT(#22396,-3.);
#9331=DERIVED_UNIT_ELEMENT(#9345,1.);
#9332=DERIVED_UNIT_ELEMENT(#22396,-3.);
#9333=DERIVED_UNIT_ELEMENT(#9345,1.);
#9334=DERIVED_UNIT_ELEMENT(#22396,-3.);
#9335=DERIVED_UNIT_ELEMENT(#9345,1.);
#9336=DERIVED_UNIT_ELEMENT(#22396,-3.);
#9337=DERIVED_UNIT_ELEMENT(#9345,1.);
#9338=DERIVED_UNIT_ELEMENT(#22396,-3.);
#9339=DERIVED_UNIT_ELEMENT(#9345,1.);
#9340=DERIVED_UNIT_ELEMENT(#22396,-3.);
#9341=DERIVED_UNIT_ELEMENT(#9345,1.);
#9342=DERIVED_UNIT_ELEMENT(#22396,-3.);
#9343=DERIVED_UNIT_ELEMENT(#9345,1.);
#9344=DERIVED_UNIT_ELEMENT(#22396,-3.);
#9345=(
MASS_UNIT()
NAMED_UNIT(*)
SI_UNIT(.KILO.,.GRAM.)
);
#9346=DERIVED_UNIT((#9253,#9254));
#9347=DERIVED_UNIT((#9255,#9256));
#9348=DERIVED_UNIT((#9257,#9258));
#9349=DERIVED_UNIT((#9259,#9260));
#9350=DERIVED_UNIT((#9261,#9262));
#9351=DERIVED_UNIT((#9263,#9264));
#9352=DERIVED_UNIT((#9265,#9266));
#9353=DERIVED_UNIT((#9267,#9268));
#9354=DERIVED_UNIT((#9269,#9270));
#9355=DERIVED_UNIT((#9271,#9272));
#9356=DERIVED_UNIT((#9273,#9274));
#9357=DERIVED_UNIT((#9275,#9276));
#9358=DERIVED_UNIT((#9277,#9278));
#9359=DERIVED_UNIT((#9279,#9280));
#9360=DERIVED_UNIT((#9281,#9282));
#9361=DERIVED_UNIT((#9283,#9284));
#9362=DERIVED_UNIT((#9285,#9286));
#9363=DERIVED_UNIT((#9287,#9288));
#9364=DERIVED_UNIT((#9289,#9290));
#9365=DERIVED_UNIT((#9291,#9292));
#9366=DERIVED_UNIT((#9293,#9294));
#9367=DERIVED_UNIT((#9295,#9296));
#9368=DERIVED_UNIT((#9297,#9298));
#9369=DERIVED_UNIT((#9299,#9300));
#9370=DERIVED_UNIT((#9301,#9302));
#9371=DERIVED_UNIT((#9303,#9304));
#9372=DERIVED_UNIT((#9305,#9306));
#9373=DERIVED_UNIT((#9307,#9308));
#9374=DERIVED_UNIT((#9309,#9310));
#9375=DERIVED_UNIT((#9311,#9312));
#9376=DERIVED_UNIT((#9313,#9314));
#9377=DERIVED_UNIT((#9315,#9316));
#9378=DERIVED_UNIT((#9317,#9318));
#9379=DERIVED_UNIT((#9319,#9320));
#9380=DERIVED_UNIT((#9321,#9322));
#9381=DERIVED_UNIT((#9323,#9324));
#9382=DERIVED_UNIT((#9325,#9326));
#9383=DERIVED_UNIT((#9327,#9328));
#9384=DERIVED_UNIT((#9329,#9330));
#9385=DERIVED_UNIT((#9331,#9332));
#9386=DERIVED_UNIT((#9333,#9334));
#9387=DERIVED_UNIT((#9335,#9336));
#9388=DERIVED_UNIT((#9337,#9338));
#9389=DERIVED_UNIT((#9339,#9340));
#9390=DERIVED_UNIT((#9341,#9342));
#9391=DERIVED_UNIT((#9343,#9344));
#9392=MEASURE_REPRESENTATION_ITEM('density measure',
POSITIVE_RATIO_MEASURE(7850.),#9346);
#9393=MEASURE_REPRESENTATION_ITEM('density measure',
POSITIVE_RATIO_MEASURE(7850.),#9347);
#9394=MEASURE_REPRESENTATION_ITEM('density measure',
POSITIVE_RATIO_MEASURE(7850.),#9348);
#9395=MEASURE_REPRESENTATION_ITEM('density measure',
POSITIVE_RATIO_MEASURE(7850.),#9349);
#9396=MEASURE_REPRESENTATION_ITEM('density measure',
POSITIVE_RATIO_MEASURE(7850.),#9350);
#9397=MEASURE_REPRESENTATION_ITEM('density measure',
POSITIVE_RATIO_MEASURE(7850.),#9351);
#9398=MEASURE_REPRESENTATION_ITEM('density measure',
POSITIVE_RATIO_MEASURE(7850.),#9352);
#9399=MEASURE_REPRESENTATION_ITEM('density measure',
POSITIVE_RATIO_MEASURE(7850.),#9353);
#9400=MEASURE_REPRESENTATION_ITEM('density measure',
POSITIVE_RATIO_MEASURE(7850.),#9354);
#9401=MEASURE_REPRESENTATION_ITEM('density measure',
POSITIVE_RATIO_MEASURE(7850.),#9355);
#9402=MEASURE_REPRESENTATION_ITEM('density measure',
POSITIVE_RATIO_MEASURE(7850.),#9356);
#9403=MEASURE_REPRESENTATION_ITEM('density measure',
POSITIVE_RATIO_MEASURE(7850.),#9357);
#9404=MEASURE_REPRESENTATION_ITEM('density measure',
POSITIVE_RATIO_MEASURE(7850.),#9358);
#9405=MEASURE_REPRESENTATION_ITEM('density measure',
POSITIVE_RATIO_MEASURE(7850.),#9359);
#9406=MEASURE_REPRESENTATION_ITEM('density measure',
POSITIVE_RATIO_MEASURE(7850.),#9360);
#9407=MEASURE_REPRESENTATION_ITEM('density measure',
POSITIVE_RATIO_MEASURE(7850.),#9361);
#9408=MEASURE_REPRESENTATION_ITEM('density measure',
POSITIVE_RATIO_MEASURE(7850.),#9362);
#9409=MEASURE_REPRESENTATION_ITEM('density measure',
POSITIVE_RATIO_MEASURE(7850.),#9363);
#9410=MEASURE_REPRESENTATION_ITEM('density measure',
POSITIVE_RATIO_MEASURE(7850.),#9364);
#9411=MEASURE_REPRESENTATION_ITEM('density measure',
POSITIVE_RATIO_MEASURE(7850.),#9365);
#9412=MEASURE_REPRESENTATION_ITEM('density measure',
POSITIVE_RATIO_MEASURE(7850.),#9366);
#9413=MEASURE_REPRESENTATION_ITEM('density measure',
POSITIVE_RATIO_MEASURE(7850.),#9367);
#9414=MEASURE_REPRESENTATION_ITEM('density measure',
POSITIVE_RATIO_MEASURE(7850.),#9368);
#9415=MEASURE_REPRESENTATION_ITEM('density measure',
POSITIVE_RATIO_MEASURE(7850.),#9369);
#9416=MEASURE_REPRESENTATION_ITEM('density measure',
POSITIVE_RATIO_MEASURE(7850.),#9370);
#9417=MEASURE_REPRESENTATION_ITEM('density measure',
POSITIVE_RATIO_MEASURE(7850.),#9371);
#9418=MEASURE_REPRESENTATION_ITEM('density measure',
POSITIVE_RATIO_MEASURE(7850.),#9372);
#9419=MEASURE_REPRESENTATION_ITEM('density measure',
POSITIVE_RATIO_MEASURE(7850.),#9373);
#9420=MEASURE_REPRESENTATION_ITEM('density measure',
POSITIVE_RATIO_MEASURE(7850.),#9374);
#9421=MEASURE_REPRESENTATION_ITEM('density measure',
POSITIVE_RATIO_MEASURE(7850.),#9375);
#9422=MEASURE_REPRESENTATION_ITEM('density measure',
POSITIVE_RATIO_MEASURE(7850.),#9376);
#9423=MEASURE_REPRESENTATION_ITEM('density measure',
POSITIVE_RATIO_MEASURE(7850.),#9377);
#9424=MEASURE_REPRESENTATION_ITEM('density measure',
POSITIVE_RATIO_MEASURE(7850.),#9378);
#9425=MEASURE_REPRESENTATION_ITEM('density measure',
POSITIVE_RATIO_MEASURE(7850.),#9379);
#9426=MEASURE_REPRESENTATION_ITEM('density measure',
POSITIVE_RATIO_MEASURE(7850.),#9380);
#9427=MEASURE_REPRESENTATION_ITEM('density measure',
POSITIVE_RATIO_MEASURE(7850.),#9381);
#9428=MEASURE_REPRESENTATION_ITEM('density measure',
POSITIVE_RATIO_MEASURE(7850.),#9382);
#9429=MEASURE_REPRESENTATION_ITEM('density measure',
POSITIVE_RATIO_MEASURE(7850.),#9383);
#9430=MEASURE_REPRESENTATION_ITEM('density measure',
POSITIVE_RATIO_MEASURE(7850.),#9384);
#9431=MEASURE_REPRESENTATION_ITEM('density measure',
POSITIVE_RATIO_MEASURE(7850.),#9385);
#9432=MEASURE_REPRESENTATION_ITEM('density measure',
POSITIVE_RATIO_MEASURE(7850.),#9386);
#9433=MEASURE_REPRESENTATION_ITEM('density measure',
POSITIVE_RATIO_MEASURE(7850.),#9387);
#9434=MEASURE_REPRESENTATION_ITEM('density measure',
POSITIVE_RATIO_MEASURE(7850.),#9388);
#9435=MEASURE_REPRESENTATION_ITEM('density measure',
POSITIVE_RATIO_MEASURE(7850.),#9389);
#9436=MEASURE_REPRESENTATION_ITEM('density measure',
POSITIVE_RATIO_MEASURE(7850.),#9390);
#9437=MEASURE_REPRESENTATION_ITEM('density measure',
POSITIVE_RATIO_MEASURE(7850.),#9391);
#9438=PROPERTY_DEFINITION_REPRESENTATION(#9668,#9530);
#9439=PROPERTY_DEFINITION_REPRESENTATION(#9669,#9531);
#9440=PROPERTY_DEFINITION_REPRESENTATION(#9670,#9532);
#9441=PROPERTY_DEFINITION_REPRESENTATION(#9671,#9533);
#9442=PROPERTY_DEFINITION_REPRESENTATION(#9672,#9534);
#9443=PROPERTY_DEFINITION_REPRESENTATION(#9673,#9535);
#9444=PROPERTY_DEFINITION_REPRESENTATION(#9674,#9536);
#9445=PROPERTY_DEFINITION_REPRESENTATION(#9675,#9537);
#9446=PROPERTY_DEFINITION_REPRESENTATION(#9676,#9538);
#9447=PROPERTY_DEFINITION_REPRESENTATION(#9677,#9539);
#9448=PROPERTY_DEFINITION_REPRESENTATION(#9678,#9540);
#9449=PROPERTY_DEFINITION_REPRESENTATION(#9679,#9541);
#9450=PROPERTY_DEFINITION_REPRESENTATION(#9680,#9542);
#9451=PROPERTY_DEFINITION_REPRESENTATION(#9681,#9543);
#9452=PROPERTY_DEFINITION_REPRESENTATION(#9682,#9544);
#9453=PROPERTY_DEFINITION_REPRESENTATION(#9683,#9545);
#9454=PROPERTY_DEFINITION_REPRESENTATION(#9684,#9546);
#9455=PROPERTY_DEFINITION_REPRESENTATION(#9685,#9547);
#9456=PROPERTY_DEFINITION_REPRESENTATION(#9686,#9548);
#9457=PROPERTY_DEFINITION_REPRESENTATION(#9687,#9549);
#9458=PROPERTY_DEFINITION_REPRESENTATION(#9688,#9550);
#9459=PROPERTY_DEFINITION_REPRESENTATION(#9689,#9551);
#9460=PROPERTY_DEFINITION_REPRESENTATION(#9690,#9552);
#9461=PROPERTY_DEFINITION_REPRESENTATION(#9691,#9553);
#9462=PROPERTY_DEFINITION_REPRESENTATION(#9692,#9554);
#9463=PROPERTY_DEFINITION_REPRESENTATION(#9693,#9555);
#9464=PROPERTY_DEFINITION_REPRESENTATION(#9694,#9556);
#9465=PROPERTY_DEFINITION_REPRESENTATION(#9695,#9557);
#9466=PROPERTY_DEFINITION_REPRESENTATION(#9696,#9558);
#9467=PROPERTY_DEFINITION_REPRESENTATION(#9697,#9559);
#9468=PROPERTY_DEFINITION_REPRESENTATION(#9698,#9560);
#9469=PROPERTY_DEFINITION_REPRESENTATION(#9699,#9561);
#9470=PROPERTY_DEFINITION_REPRESENTATION(#9700,#9562);
#9471=PROPERTY_DEFINITION_REPRESENTATION(#9701,#9563);
#9472=PROPERTY_DEFINITION_REPRESENTATION(#9702,#9564);
#9473=PROPERTY_DEFINITION_REPRESENTATION(#9703,#9565);
#9474=PROPERTY_DEFINITION_REPRESENTATION(#9704,#9566);
#9475=PROPERTY_DEFINITION_REPRESENTATION(#9705,#9567);
#9476=PROPERTY_DEFINITION_REPRESENTATION(#9706,#9568);
#9477=PROPERTY_DEFINITION_REPRESENTATION(#9707,#9569);
#9478=PROPERTY_DEFINITION_REPRESENTATION(#9708,#9570);
#9479=PROPERTY_DEFINITION_REPRESENTATION(#9709,#9571);
#9480=PROPERTY_DEFINITION_REPRESENTATION(#9710,#9572);
#9481=PROPERTY_DEFINITION_REPRESENTATION(#9711,#9573);
#9482=PROPERTY_DEFINITION_REPRESENTATION(#9712,#9574);
#9483=PROPERTY_DEFINITION_REPRESENTATION(#9713,#9575);
#9484=PROPERTY_DEFINITION_REPRESENTATION(#9714,#9576);
#9485=PROPERTY_DEFINITION_REPRESENTATION(#9715,#9577);
#9486=PROPERTY_DEFINITION_REPRESENTATION(#9716,#9578);
#9487=PROPERTY_DEFINITION_REPRESENTATION(#9717,#9579);
#9488=PROPERTY_DEFINITION_REPRESENTATION(#9718,#9580);
#9489=PROPERTY_DEFINITION_REPRESENTATION(#9719,#9581);
#9490=PROPERTY_DEFINITION_REPRESENTATION(#9720,#9582);
#9491=PROPERTY_DEFINITION_REPRESENTATION(#9721,#9583);
#9492=PROPERTY_DEFINITION_REPRESENTATION(#9722,#9584);
#9493=PROPERTY_DEFINITION_REPRESENTATION(#9723,#9585);
#9494=PROPERTY_DEFINITION_REPRESENTATION(#9724,#9586);
#9495=PROPERTY_DEFINITION_REPRESENTATION(#9725,#9587);
#9496=PROPERTY_DEFINITION_REPRESENTATION(#9726,#9588);
#9497=PROPERTY_DEFINITION_REPRESENTATION(#9727,#9589);
#9498=PROPERTY_DEFINITION_REPRESENTATION(#9728,#9590);
#9499=PROPERTY_DEFINITION_REPRESENTATION(#9729,#9591);
#9500=PROPERTY_DEFINITION_REPRESENTATION(#9730,#9592);
#9501=PROPERTY_DEFINITION_REPRESENTATION(#9731,#9593);
#9502=PROPERTY_DEFINITION_REPRESENTATION(#9732,#9594);
#9503=PROPERTY_DEFINITION_REPRESENTATION(#9733,#9595);
#9504=PROPERTY_DEFINITION_REPRESENTATION(#9734,#9596);
#9505=PROPERTY_DEFINITION_REPRESENTATION(#9735,#9597);
#9506=PROPERTY_DEFINITION_REPRESENTATION(#9736,#9598);
#9507=PROPERTY_DEFINITION_REPRESENTATION(#9737,#9599);
#9508=PROPERTY_DEFINITION_REPRESENTATION(#9738,#9600);
#9509=PROPERTY_DEFINITION_REPRESENTATION(#9739,#9601);
#9510=PROPERTY_DEFINITION_REPRESENTATION(#9740,#9602);
#9511=PROPERTY_DEFINITION_REPRESENTATION(#9741,#9603);
#9512=PROPERTY_DEFINITION_REPRESENTATION(#9742,#9604);
#9513=PROPERTY_DEFINITION_REPRESENTATION(#9743,#9605);
#9514=PROPERTY_DEFINITION_REPRESENTATION(#9744,#9606);
#9515=PROPERTY_DEFINITION_REPRESENTATION(#9745,#9607);
#9516=PROPERTY_DEFINITION_REPRESENTATION(#9746,#9608);
#9517=PROPERTY_DEFINITION_REPRESENTATION(#9747,#9609);
#9518=PROPERTY_DEFINITION_REPRESENTATION(#9748,#9610);
#9519=PROPERTY_DEFINITION_REPRESENTATION(#9749,#9611);
#9520=PROPERTY_DEFINITION_REPRESENTATION(#9750,#9612);
#9521=PROPERTY_DEFINITION_REPRESENTATION(#9751,#9613);
#9522=PROPERTY_DEFINITION_REPRESENTATION(#9752,#9614);
#9523=PROPERTY_DEFINITION_REPRESENTATION(#9753,#9615);
#9524=PROPERTY_DEFINITION_REPRESENTATION(#9754,#9616);
#9525=PROPERTY_DEFINITION_REPRESENTATION(#9755,#9617);
#9526=PROPERTY_DEFINITION_REPRESENTATION(#9756,#9618);
#9527=PROPERTY_DEFINITION_REPRESENTATION(#9757,#9619);
#9528=PROPERTY_DEFINITION_REPRESENTATION(#9758,#9620);
#9529=PROPERTY_DEFINITION_REPRESENTATION(#9759,#9621);
#9530=REPRESENTATION('material name',(#9622),#22346);
#9531=REPRESENTATION('density',(#9392),#22346);
#9532=REPRESENTATION('material name',(#9623),#22347);
#9533=REPRESENTATION('density',(#9393),#22347);
#9534=REPRESENTATION('material name',(#9624),#22348);
#9535=REPRESENTATION('density',(#9394),#22348);
#9536=REPRESENTATION('material name',(#9625),#22349);
#9537=REPRESENTATION('density',(#9395),#22349);
#9538=REPRESENTATION('material name',(#9626),#22350);
#9539=REPRESENTATION('density',(#9396),#22350);
#9540=REPRESENTATION('material name',(#9627),#22351);
#9541=REPRESENTATION('density',(#9397),#22351);
#9542=REPRESENTATION('material name',(#9628),#22352);
#9543=REPRESENTATION('density',(#9398),#22352);
#9544=REPRESENTATION('material name',(#9629),#22353);
#9545=REPRESENTATION('density',(#9399),#22353);
#9546=REPRESENTATION('material name',(#9630),#22354);
#9547=REPRESENTATION('density',(#9400),#22354);
#9548=REPRESENTATION('material name',(#9631),#22355);
#9549=REPRESENTATION('density',(#9401),#22355);
#9550=REPRESENTATION('material name',(#9632),#22356);
#9551=REPRESENTATION('density',(#9402),#22356);
#9552=REPRESENTATION('material name',(#9633),#22357);
#9553=REPRESENTATION('density',(#9403),#22357);
#9554=REPRESENTATION('material name',(#9634),#22358);
#9555=REPRESENTATION('density',(#9404),#22358);
#9556=REPRESENTATION('material name',(#9635),#22359);
#9557=REPRESENTATION('density',(#9405),#22359);
#9558=REPRESENTATION('material name',(#9636),#22360);
#9559=REPRESENTATION('density',(#9406),#22360);
#9560=REPRESENTATION('material name',(#9637),#22361);
#9561=REPRESENTATION('density',(#9407),#22361);
#9562=REPRESENTATION('material name',(#9638),#22362);
#9563=REPRESENTATION('density',(#9408),#22362);
#9564=REPRESENTATION('material name',(#9639),#22363);
#9565=REPRESENTATION('density',(#9409),#22363);
#9566=REPRESENTATION('material name',(#9640),#22364);
#9567=REPRESENTATION('density',(#9410),#22364);
#9568=REPRESENTATION('material name',(#9641),#22365);
#9569=REPRESENTATION('density',(#9411),#22365);
#9570=REPRESENTATION('material name',(#9642),#22366);
#9571=REPRESENTATION('density',(#9412),#22366);
#9572=REPRESENTATION('material name',(#9643),#22367);
#9573=REPRESENTATION('density',(#9413),#22367);
#9574=REPRESENTATION('material name',(#9644),#22368);
#9575=REPRESENTATION('density',(#9414),#22368);
#9576=REPRESENTATION('material name',(#9645),#22369);
#9577=REPRESENTATION('density',(#9415),#22369);
#9578=REPRESENTATION('material name',(#9646),#22370);
#9579=REPRESENTATION('density',(#9416),#22370);
#9580=REPRESENTATION('material name',(#9647),#22371);
#9581=REPRESENTATION('density',(#9417),#22371);
#9582=REPRESENTATION('material name',(#9648),#22372);
#9583=REPRESENTATION('density',(#9418),#22372);
#9584=REPRESENTATION('material name',(#9649),#22373);
#9585=REPRESENTATION('density',(#9419),#22373);
#9586=REPRESENTATION('material name',(#9650),#22374);
#9587=REPRESENTATION('density',(#9420),#22374);
#9588=REPRESENTATION('material name',(#9651),#22375);
#9589=REPRESENTATION('density',(#9421),#22375);
#9590=REPRESENTATION('material name',(#9652),#22376);
#9591=REPRESENTATION('density',(#9422),#22376);
#9592=REPRESENTATION('material name',(#9653),#22377);
#9593=REPRESENTATION('density',(#9423),#22377);
#9594=REPRESENTATION('material name',(#9654),#22378);
#9595=REPRESENTATION('density',(#9424),#22378);
#9596=REPRESENTATION('material name',(#9655),#22379);
#9597=REPRESENTATION('density',(#9425),#22379);
#9598=REPRESENTATION('material name',(#9656),#22380);
#9599=REPRESENTATION('density',(#9426),#22380);
#9600=REPRESENTATION('material name',(#9657),#22381);
#9601=REPRESENTATION('density',(#9427),#22381);
#9602=REPRESENTATION('material name',(#9658),#22382);
#9603=REPRESENTATION('density',(#9428),#22382);
#9604=REPRESENTATION('material name',(#9659),#22384);
#9605=REPRESENTATION('density',(#9429),#22384);
#9606=REPRESENTATION('material name',(#9660),#22385);
#9607=REPRESENTATION('density',(#9430),#22385);
#9608=REPRESENTATION('material name',(#9661),#22386);
#9609=REPRESENTATION('density',(#9431),#22386);
#9610=REPRESENTATION('material name',(#9662),#22387);
#9611=REPRESENTATION('density',(#9432),#22387);
#9612=REPRESENTATION('material name',(#9663),#22388);
#9613=REPRESENTATION('density',(#9433),#22388);
#9614=REPRESENTATION('material name',(#9664),#22389);
#9615=REPRESENTATION('density',(#9434),#22389);
#9616=REPRESENTATION('material name',(#9665),#22391);
#9617=REPRESENTATION('density',(#9435),#22391);
#9618=REPRESENTATION('material name',(#9666),#22392);
#9619=REPRESENTATION('density',(#9436),#22392);
#9620=REPRESENTATION('material name',(#9667),#22393);
#9621=REPRESENTATION('density',(#9437),#22393);
#9622=DESCRIPTIVE_REPRESENTATION_ITEM('Steel','Steel');
#9623=DESCRIPTIVE_REPRESENTATION_ITEM('Steel','Steel');
#9624=DESCRIPTIVE_REPRESENTATION_ITEM('Steel','Steel');
#9625=DESCRIPTIVE_REPRESENTATION_ITEM('Steel','Steel');
#9626=DESCRIPTIVE_REPRESENTATION_ITEM('Steel','Steel');
#9627=DESCRIPTIVE_REPRESENTATION_ITEM('Steel','Steel');
#9628=DESCRIPTIVE_REPRESENTATION_ITEM('Steel','Steel');
#9629=DESCRIPTIVE_REPRESENTATION_ITEM('Steel','Steel');
#9630=DESCRIPTIVE_REPRESENTATION_ITEM('Steel','Steel');
#9631=DESCRIPTIVE_REPRESENTATION_ITEM('Steel','Steel');
#9632=DESCRIPTIVE_REPRESENTATION_ITEM('Steel','Steel');
#9633=DESCRIPTIVE_REPRESENTATION_ITEM('Steel','Steel');
#9634=DESCRIPTIVE_REPRESENTATION_ITEM('Steel','Steel');
#9635=DESCRIPTIVE_REPRESENTATION_ITEM('Steel','Steel');
#9636=DESCRIPTIVE_REPRESENTATION_ITEM('Steel','Steel');
#9637=DESCRIPTIVE_REPRESENTATION_ITEM('Steel','Steel');
#9638=DESCRIPTIVE_REPRESENTATION_ITEM('Steel','Steel');
#9639=DESCRIPTIVE_REPRESENTATION_ITEM('Steel','Steel');
#9640=DESCRIPTIVE_REPRESENTATION_ITEM('Steel','Steel');
#9641=DESCRIPTIVE_REPRESENTATION_ITEM('Steel','Steel');
#9642=DESCRIPTIVE_REPRESENTATION_ITEM('Steel','Steel');
#9643=DESCRIPTIVE_REPRESENTATION_ITEM('Steel','Steel');
#9644=DESCRIPTIVE_REPRESENTATION_ITEM('Steel','Steel');
#9645=DESCRIPTIVE_REPRESENTATION_ITEM('Steel','Steel');
#9646=DESCRIPTIVE_REPRESENTATION_ITEM('Steel','Steel');
#9647=DESCRIPTIVE_REPRESENTATION_ITEM('Steel','Steel');
#9648=DESCRIPTIVE_REPRESENTATION_ITEM('Steel','Steel');
#9649=DESCRIPTIVE_REPRESENTATION_ITEM('Steel','Steel');
#9650=DESCRIPTIVE_REPRESENTATION_ITEM('Steel','Steel');
#9651=DESCRIPTIVE_REPRESENTATION_ITEM('Steel','Steel');
#9652=DESCRIPTIVE_REPRESENTATION_ITEM('Steel','Steel');
#9653=DESCRIPTIVE_REPRESENTATION_ITEM('Steel','Steel');
#9654=DESCRIPTIVE_REPRESENTATION_ITEM('Steel','Steel');
#9655=DESCRIPTIVE_REPRESENTATION_ITEM('Steel','Steel');
#9656=DESCRIPTIVE_REPRESENTATION_ITEM('Steel','Steel');
#9657=DESCRIPTIVE_REPRESENTATION_ITEM('Steel','Steel');
#9658=DESCRIPTIVE_REPRESENTATION_ITEM('Steel','Steel');
#9659=DESCRIPTIVE_REPRESENTATION_ITEM('Steel','Steel');
#9660=DESCRIPTIVE_REPRESENTATION_ITEM('Steel','Steel');
#9661=DESCRIPTIVE_REPRESENTATION_ITEM('Steel','Steel');
#9662=DESCRIPTIVE_REPRESENTATION_ITEM('Steel','Steel');
#9663=DESCRIPTIVE_REPRESENTATION_ITEM('Steel','Steel');
#9664=DESCRIPTIVE_REPRESENTATION_ITEM('Steel','Steel');
#9665=DESCRIPTIVE_REPRESENTATION_ITEM('Steel','Steel');
#9666=DESCRIPTIVE_REPRESENTATION_ITEM('Steel','Steel');
#9667=DESCRIPTIVE_REPRESENTATION_ITEM('Steel','Steel');
#9668=PROPERTY_DEFINITION('material property','material name',#22691);
#9669=PROPERTY_DEFINITION('material property','density of part',#22691);
#9670=PROPERTY_DEFINITION('material property','material name',#22692);
#9671=PROPERTY_DEFINITION('material property','density of part',#22692);
#9672=PROPERTY_DEFINITION('material property','material name',#22693);
#9673=PROPERTY_DEFINITION('material property','density of part',#22693);
#9674=PROPERTY_DEFINITION('material property','material name',#22694);
#9675=PROPERTY_DEFINITION('material property','density of part',#22694);
#9676=PROPERTY_DEFINITION('material property','material name',#22695);
#9677=PROPERTY_DEFINITION('material property','density of part',#22695);
#9678=PROPERTY_DEFINITION('material property','material name',#22696);
#9679=PROPERTY_DEFINITION('material property','density of part',#22696);
#9680=PROPERTY_DEFINITION('material property','material name',#22697);
#9681=PROPERTY_DEFINITION('material property','density of part',#22697);
#9682=PROPERTY_DEFINITION('material property','material name',#22698);
#9683=PROPERTY_DEFINITION('material property','density of part',#22698);
#9684=PROPERTY_DEFINITION('material property','material name',#22699);
#9685=PROPERTY_DEFINITION('material property','density of part',#22699);
#9686=PROPERTY_DEFINITION('material property','material name',#22700);
#9687=PROPERTY_DEFINITION('material property','density of part',#22700);
#9688=PROPERTY_DEFINITION('material property','material name',#22701);
#9689=PROPERTY_DEFINITION('material property','density of part',#22701);
#9690=PROPERTY_DEFINITION('material property','material name',#22702);
#9691=PROPERTY_DEFINITION('material property','density of part',#22702);
#9692=PROPERTY_DEFINITION('material property','material name',#22703);
#9693=PROPERTY_DEFINITION('material property','density of part',#22703);
#9694=PROPERTY_DEFINITION('material property','material name',#22704);
#9695=PROPERTY_DEFINITION('material property','density of part',#22704);
#9696=PROPERTY_DEFINITION('material property','material name',#22705);
#9697=PROPERTY_DEFINITION('material property','density of part',#22705);
#9698=PROPERTY_DEFINITION('material property','material name',#22706);
#9699=PROPERTY_DEFINITION('material property','density of part',#22706);
#9700=PROPERTY_DEFINITION('material property','material name',#22707);
#9701=PROPERTY_DEFINITION('material property','density of part',#22707);
#9702=PROPERTY_DEFINITION('material property','material name',#22708);
#9703=PROPERTY_DEFINITION('material property','density of part',#22708);
#9704=PROPERTY_DEFINITION('material property','material name',#22709);
#9705=PROPERTY_DEFINITION('material property','density of part',#22709);
#9706=PROPERTY_DEFINITION('material property','material name',#22710);
#9707=PROPERTY_DEFINITION('material property','density of part',#22710);
#9708=PROPERTY_DEFINITION('material property','material name',#22711);
#9709=PROPERTY_DEFINITION('material property','density of part',#22711);
#9710=PROPERTY_DEFINITION('material property','material name',#22712);
#9711=PROPERTY_DEFINITION('material property','density of part',#22712);
#9712=PROPERTY_DEFINITION('material property','material name',#22713);
#9713=PROPERTY_DEFINITION('material property','density of part',#22713);
#9714=PROPERTY_DEFINITION('material property','material name',#22714);
#9715=PROPERTY_DEFINITION('material property','density of part',#22714);
#9716=PROPERTY_DEFINITION('material property','material name',#22715);
#9717=PROPERTY_DEFINITION('material property','density of part',#22715);
#9718=PROPERTY_DEFINITION('material property','material name',#22716);
#9719=PROPERTY_DEFINITION('material property','density of part',#22716);
#9720=PROPERTY_DEFINITION('material property','material name',#22717);
#9721=PROPERTY_DEFINITION('material property','density of part',#22717);
#9722=PROPERTY_DEFINITION('material property','material name',#22718);
#9723=PROPERTY_DEFINITION('material property','density of part',#22718);
#9724=PROPERTY_DEFINITION('material property','material name',#22719);
#9725=PROPERTY_DEFINITION('material property','density of part',#22719);
#9726=PROPERTY_DEFINITION('material property','material name',#22720);
#9727=PROPERTY_DEFINITION('material property','density of part',#22720);
#9728=PROPERTY_DEFINITION('material property','material name',#22721);
#9729=PROPERTY_DEFINITION('material property','density of part',#22721);
#9730=PROPERTY_DEFINITION('material property','material name',#22722);
#9731=PROPERTY_DEFINITION('material property','density of part',#22722);
#9732=PROPERTY_DEFINITION('material property','material name',#22723);
#9733=PROPERTY_DEFINITION('material property','density of part',#22723);
#9734=PROPERTY_DEFINITION('material property','material name',#22724);
#9735=PROPERTY_DEFINITION('material property','density of part',#22724);
#9736=PROPERTY_DEFINITION('material property','material name',#22725);
#9737=PROPERTY_DEFINITION('material property','density of part',#22725);
#9738=PROPERTY_DEFINITION('material property','material name',#22726);
#9739=PROPERTY_DEFINITION('material property','density of part',#22726);
#9740=PROPERTY_DEFINITION('material property','material name',#22727);
#9741=PROPERTY_DEFINITION('material property','density of part',#22727);
#9742=PROPERTY_DEFINITION('material property','material name',#22729);
#9743=PROPERTY_DEFINITION('material property','density of part',#22729);
#9744=PROPERTY_DEFINITION('material property','material name',#22730);
#9745=PROPERTY_DEFINITION('material property','density of part',#22730);
#9746=PROPERTY_DEFINITION('material property','material name',#22731);
#9747=PROPERTY_DEFINITION('material property','density of part',#22731);
#9748=PROPERTY_DEFINITION('material property','material name',#22732);
#9749=PROPERTY_DEFINITION('material property','density of part',#22732);
#9750=PROPERTY_DEFINITION('material property','material name',#22733);
#9751=PROPERTY_DEFINITION('material property','density of part',#22733);
#9752=PROPERTY_DEFINITION('material property','material name',#22734);
#9753=PROPERTY_DEFINITION('material property','density of part',#22734);
#9754=PROPERTY_DEFINITION('material property','material name',#22736);
#9755=PROPERTY_DEFINITION('material property','density of part',#22736);
#9756=PROPERTY_DEFINITION('material property','material name',#22737);
#9757=PROPERTY_DEFINITION('material property','density of part',#22737);
#9758=PROPERTY_DEFINITION('material property','material name',#22738);
#9759=PROPERTY_DEFINITION('material property','density of part',#22738);
#9760=AXIS2_PLACEMENT_3D('',#13949,#10950,#10951);
#9761=AXIS2_PLACEMENT_3D('',#13950,#10952,#10953);
#9762=AXIS2_PLACEMENT_3D('',#13951,#10954,#10955);
#9763=AXIS2_PLACEMENT_3D('',#13952,#10956,#10957);
#9764=AXIS2_PLACEMENT_3D('',#13954,#10958,#10959);
#9765=AXIS2_PLACEMENT_3D('',#13957,#10961,#10962);
#9766=AXIS2_PLACEMENT_3D('',#13958,#10963,#10964);
#9767=AXIS2_PLACEMENT_3D('',#13960,#10965,#10966);
#9768=AXIS2_PLACEMENT_3D('',#13963,#10968,#10969);
#9769=AXIS2_PLACEMENT_3D('',#13964,#10970,#10971);
#9770=AXIS2_PLACEMENT_3D('',#13966,#10972,#10973);
#9771=AXIS2_PLACEMENT_3D('',#13969,#10975,#10976);
#9772=AXIS2_PLACEMENT_3D('',#13970,#10977,#10978);
#9773=AXIS2_PLACEMENT_3D('',#13972,#10979,#10980);
#9774=AXIS2_PLACEMENT_3D('',#13975,#10982,#10983);
#9775=AXIS2_PLACEMENT_3D('',#13976,#10984,#10985);
#9776=AXIS2_PLACEMENT_3D('',#13978,#10986,#10987);
#9777=AXIS2_PLACEMENT_3D('',#13981,#10989,#10990);
#9778=AXIS2_PLACEMENT_3D('',#13982,#10991,#10992);
#9779=AXIS2_PLACEMENT_3D('',#13984,#10993,#10994);
#9780=AXIS2_PLACEMENT_3D('',#13987,#10996,#10997);
#9781=AXIS2_PLACEMENT_3D('',#13988,#10998,#10999);
#9782=AXIS2_PLACEMENT_3D('',#13990,#11000,#11001);
#9783=AXIS2_PLACEMENT_3D('',#13993,#11003,#11004);
#9784=AXIS2_PLACEMENT_3D('',#13994,#11005,#11006);
#9785=AXIS2_PLACEMENT_3D('',#13996,#11007,#11008);
#9786=AXIS2_PLACEMENT_3D('',#13999,#11010,#11011);
#9787=AXIS2_PLACEMENT_3D('',#14000,#11012,#11013);
#9788=AXIS2_PLACEMENT_3D('',#14002,#11014,#11015);
#9789=AXIS2_PLACEMENT_3D('',#14005,#11017,#11018);
#9790=AXIS2_PLACEMENT_3D('',#14006,#11019,#11020);
#9791=AXIS2_PLACEMENT_3D('',#14008,#11021,#11022);
#9792=AXIS2_PLACEMENT_3D('',#14011,#11024,#11025);
#9793=AXIS2_PLACEMENT_3D('',#14012,#11026,#11027);
#9794=AXIS2_PLACEMENT_3D('',#14014,#11028,#11029);
#9795=AXIS2_PLACEMENT_3D('',#14017,#11031,#11032);
#9796=AXIS2_PLACEMENT_3D('',#14018,#11033,#11034);
#9797=AXIS2_PLACEMENT_3D('',#14020,#11035,#11036);
#9798=AXIS2_PLACEMENT_3D('',#14023,#11038,#11039);
#9799=AXIS2_PLACEMENT_3D('',#14024,#11040,#11041);
#9800=AXIS2_PLACEMENT_3D('',#14026,#11042,#11043);
#9801=AXIS2_PLACEMENT_3D('',#14029,#11045,#11046);
#9802=AXIS2_PLACEMENT_3D('',#14030,#11047,#11048);
#9803=AXIS2_PLACEMENT_3D('',#14032,#11049,#11050);
#9804=AXIS2_PLACEMENT_3D('',#14035,#11052,#11053);
#9805=AXIS2_PLACEMENT_3D('',#14036,#11054,#11055);
#9806=AXIS2_PLACEMENT_3D('',#14038,#11056,#11057);
#9807=AXIS2_PLACEMENT_3D('',#14041,#11059,#11060);
#9808=AXIS2_PLACEMENT_3D('',#14042,#11061,#11062);
#9809=AXIS2_PLACEMENT_3D('',#14044,#11063,#11064);
#9810=AXIS2_PLACEMENT_3D('',#14047,#11066,#11067);
#9811=AXIS2_PLACEMENT_3D('',#14048,#11068,#11069);
#9812=AXIS2_PLACEMENT_3D('',#14050,#11070,#11071);
#9813=AXIS2_PLACEMENT_3D('',#14053,#11073,#11074);
#9814=AXIS2_PLACEMENT_3D('',#14054,#11075,#11076);
#9815=AXIS2_PLACEMENT_3D('',#14056,#11077,#11078);
#9816=AXIS2_PLACEMENT_3D('',#14059,#11080,#11081);
#9817=AXIS2_PLACEMENT_3D('',#14060,#11082,#11083);
#9818=AXIS2_PLACEMENT_3D('',#14062,#11084,#11085);
#9819=AXIS2_PLACEMENT_3D('',#14065,#11087,#11088);
#9820=AXIS2_PLACEMENT_3D('',#14066,#11089,#11090);
#9821=AXIS2_PLACEMENT_3D('',#14068,#11091,#11092);
#9822=AXIS2_PLACEMENT_3D('',#14071,#11094,#11095);
#9823=AXIS2_PLACEMENT_3D('',#14072,#11096,#11097);
#9824=AXIS2_PLACEMENT_3D('',#14074,#11098,#11099);
#9825=AXIS2_PLACEMENT_3D('',#14077,#11101,#11102);
#9826=AXIS2_PLACEMENT_3D('',#14078,#11103,#11104);
#9827=AXIS2_PLACEMENT_3D('',#14080,#11105,#11106);
#9828=AXIS2_PLACEMENT_3D('',#14083,#11108,#11109);
#9829=AXIS2_PLACEMENT_3D('',#14084,#11110,#11111);
#9830=AXIS2_PLACEMENT_3D('',#14093,#11116,#11117);
#9831=AXIS2_PLACEMENT_3D('',#14099,#11121,#11122);
#9832=AXIS2_PLACEMENT_3D('',#14105,#11126,#11127);
#9833=AXIS2_PLACEMENT_3D('',#14108,#11130,#11131);
#9834=AXIS2_PLACEMENT_3D('',#14109,#11132,#11133);
#9835=AXIS2_PLACEMENT_3D('',#14110,#11134,#11135);
#9836=AXIS2_PLACEMENT_3D('',#14111,#11136,#11137);
#9837=AXIS2_PLACEMENT_3D('',#14120,#11142,#11143);
#9838=AXIS2_PLACEMENT_3D('',#14126,#11147,#11148);
#9839=AXIS2_PLACEMENT_3D('',#14132,#11152,#11153);
#9840=AXIS2_PLACEMENT_3D('',#14135,#11156,#11157);
#9841=AXIS2_PLACEMENT_3D('',#14136,#11158,#11159);
#9842=AXIS2_PLACEMENT_3D('',#14137,#11160,#11161);
#9843=AXIS2_PLACEMENT_3D('',#14138,#11162,#11163);
#9844=AXIS2_PLACEMENT_3D('',#14147,#11168,#11169);
#9845=AXIS2_PLACEMENT_3D('',#14153,#11173,#11174);
#9846=AXIS2_PLACEMENT_3D('',#14159,#11178,#11179);
#9847=AXIS2_PLACEMENT_3D('',#14162,#11182,#11183);
#9848=AXIS2_PLACEMENT_3D('',#14163,#11184,#11185);
#9849=AXIS2_PLACEMENT_3D('',#14164,#11186,#11187);
#9850=AXIS2_PLACEMENT_3D('',#14165,#11188,#11189);
#9851=AXIS2_PLACEMENT_3D('',#14167,#11190,#11191);
#9852=AXIS2_PLACEMENT_3D('',#14170,#11193,#11194);
#9853=AXIS2_PLACEMENT_3D('',#14171,#11195,#11196);
#9854=AXIS2_PLACEMENT_3D('',#14173,#11197,#11198);
#9855=AXIS2_PLACEMENT_3D('',#14176,#11200,#11201);
#9856=AXIS2_PLACEMENT_3D('',#14177,#11202,#11203);
#9857=AXIS2_PLACEMENT_3D('',#14179,#11204,#11205);
#9858=AXIS2_PLACEMENT_3D('',#14182,#11207,#11208);
#9859=AXIS2_PLACEMENT_3D('',#14183,#11209,#11210);
#9860=AXIS2_PLACEMENT_3D('',#14185,#11211,#11212);
#9861=AXIS2_PLACEMENT_3D('',#14188,#11214,#11215);
#9862=AXIS2_PLACEMENT_3D('',#14189,#11216,#11217);
#9863=AXIS2_PLACEMENT_3D('',#14191,#11218,#11219);
#9864=AXIS2_PLACEMENT_3D('',#14194,#11221,#11222);
#9865=AXIS2_PLACEMENT_3D('',#14195,#11223,#11224);
#9866=AXIS2_PLACEMENT_3D('',#14197,#11225,#11226);
#9867=AXIS2_PLACEMENT_3D('',#14200,#11228,#11229);
#9868=AXIS2_PLACEMENT_3D('',#14201,#11230,#11231);
#9869=AXIS2_PLACEMENT_3D('',#14203,#11232,#11233);
#9870=AXIS2_PLACEMENT_3D('',#14206,#11235,#11236);
#9871=AXIS2_PLACEMENT_3D('',#14207,#11237,#11238);
#9872=AXIS2_PLACEMENT_3D('',#14209,#11239,#11240);
#9873=AXIS2_PLACEMENT_3D('',#14212,#11242,#11243);
#9874=AXIS2_PLACEMENT_3D('',#14213,#11244,#11245);
#9875=AXIS2_PLACEMENT_3D('',#14215,#11246,#11247);
#9876=AXIS2_PLACEMENT_3D('',#14218,#11249,#11250);
#9877=AXIS2_PLACEMENT_3D('',#14219,#11251,#11252);
#9878=AXIS2_PLACEMENT_3D('',#14221,#11253,#11254);
#9879=AXIS2_PLACEMENT_3D('',#14224,#11256,#11257);
#9880=AXIS2_PLACEMENT_3D('',#14225,#11258,#11259);
#9881=AXIS2_PLACEMENT_3D('',#14227,#11260,#11261);
#9882=AXIS2_PLACEMENT_3D('',#14230,#11263,#11264);
#9883=AXIS2_PLACEMENT_3D('',#14231,#11265,#11266);
#9884=AXIS2_PLACEMENT_3D('',#14233,#11267,#11268);
#9885=AXIS2_PLACEMENT_3D('',#14236,#11270,#11271);
#9886=AXIS2_PLACEMENT_3D('',#14237,#11272,#11273);
#9887=AXIS2_PLACEMENT_3D('',#14239,#11274,#11275);
#9888=AXIS2_PLACEMENT_3D('',#14242,#11277,#11278);
#9889=AXIS2_PLACEMENT_3D('',#14243,#11279,#11280);
#9890=AXIS2_PLACEMENT_3D('',#14245,#11281,#11282);
#9891=AXIS2_PLACEMENT_3D('',#14248,#11284,#11285);
#9892=AXIS2_PLACEMENT_3D('',#14249,#11286,#11287);
#9893=AXIS2_PLACEMENT_3D('',#14251,#11288,#11289);
#9894=AXIS2_PLACEMENT_3D('',#14254,#11291,#11292);
#9895=AXIS2_PLACEMENT_3D('',#14255,#11293,#11294);
#9896=AXIS2_PLACEMENT_3D('',#14257,#11295,#11296);
#9897=AXIS2_PLACEMENT_3D('',#14260,#11298,#11299);
#9898=AXIS2_PLACEMENT_3D('',#14261,#11300,#11301);
#9899=AXIS2_PLACEMENT_3D('',#14263,#11302,#11303);
#9900=AXIS2_PLACEMENT_3D('',#14266,#11305,#11306);
#9901=AXIS2_PLACEMENT_3D('',#14267,#11307,#11308);
#9902=AXIS2_PLACEMENT_3D('',#14269,#11309,#11310);
#9903=AXIS2_PLACEMENT_3D('',#14272,#11312,#11313);
#9904=AXIS2_PLACEMENT_3D('',#14273,#11314,#11315);
#9905=AXIS2_PLACEMENT_3D('',#14282,#11320,#11321);
#9906=AXIS2_PLACEMENT_3D('',#14288,#11325,#11326);
#9907=AXIS2_PLACEMENT_3D('',#14294,#11330,#11331);
#9908=AXIS2_PLACEMENT_3D('',#14297,#11334,#11335);
#9909=AXIS2_PLACEMENT_3D('',#14298,#11336,#11337);
#9910=AXIS2_PLACEMENT_3D('',#14299,#11338,#11339);
#9911=AXIS2_PLACEMENT_3D('',#14300,#11340,#11341);
#9912=AXIS2_PLACEMENT_3D('',#14302,#11342,#11343);
#9913=AXIS2_PLACEMENT_3D('',#14305,#11345,#11346);
#9914=AXIS2_PLACEMENT_3D('',#14306,#11347,#11348);
#9915=AXIS2_PLACEMENT_3D('',#14307,#11349,#11350);
#9916=AXIS2_PLACEMENT_3D('',#14309,#11351,#11352);
#9917=AXIS2_PLACEMENT_3D('',#14312,#11354,#11355);
#9918=AXIS2_PLACEMENT_3D('',#14313,#11356,#11357);
#9919=AXIS2_PLACEMENT_3D('',#14314,#11358,#11359);
#9920=AXIS2_PLACEMENT_3D('',#14316,#11360,#11361);
#9921=AXIS2_PLACEMENT_3D('',#14319,#11363,#11364);
#9922=AXIS2_PLACEMENT_3D('',#14320,#11365,#11366);
#9923=AXIS2_PLACEMENT_3D('',#14321,#11367,#11368);
#9924=AXIS2_PLACEMENT_3D('',#14323,#11369,#11370);
#9925=AXIS2_PLACEMENT_3D('',#14326,#11372,#11373);
#9926=AXIS2_PLACEMENT_3D('',#14327,#11374,#11375);
#9927=AXIS2_PLACEMENT_3D('',#14328,#11376,#11377);
#9928=AXIS2_PLACEMENT_3D('',#14337,#11382,#11383);
#9929=AXIS2_PLACEMENT_3D('',#14343,#11387,#11388);
#9930=AXIS2_PLACEMENT_3D('',#14349,#11392,#11393);
#9931=AXIS2_PLACEMENT_3D('',#14352,#11396,#11397);
#9932=AXIS2_PLACEMENT_3D('',#14353,#11398,#11399);
#9933=AXIS2_PLACEMENT_3D('',#14354,#11400,#11401);
#9934=AXIS2_PLACEMENT_3D('',#14355,#11402,#11403);
#9935=AXIS2_PLACEMENT_3D('',#14357,#11404,#11405);
#9936=AXIS2_PLACEMENT_3D('',#14360,#11407,#11408);
#9937=AXIS2_PLACEMENT_3D('',#14361,#11409,#11410);
#9938=AXIS2_PLACEMENT_3D('',#14362,#11411,#11412);
#9939=AXIS2_PLACEMENT_3D('',#14364,#11413,#11414);
#9940=AXIS2_PLACEMENT_3D('',#14367,#11416,#11417);
#9941=AXIS2_PLACEMENT_3D('',#14368,#11418,#11419);
#9942=AXIS2_PLACEMENT_3D('',#14369,#11420,#11421);
#9943=AXIS2_PLACEMENT_3D('',#14371,#11422,#11423);
#9944=AXIS2_PLACEMENT_3D('',#14374,#11425,#11426);
#9945=AXIS2_PLACEMENT_3D('',#14375,#11427,#11428);
#9946=AXIS2_PLACEMENT_3D('',#14376,#11429,#11430);
#9947=AXIS2_PLACEMENT_3D('',#14378,#11431,#11432);
#9948=AXIS2_PLACEMENT_3D('',#14381,#11434,#11435);
#9949=AXIS2_PLACEMENT_3D('',#14382,#11436,#11437);
#9950=AXIS2_PLACEMENT_3D('',#14383,#11438,#11439);
#9951=AXIS2_PLACEMENT_3D('',#14392,#11444,#11445);
#9952=AXIS2_PLACEMENT_3D('',#14398,#11449,#11450);
#9953=AXIS2_PLACEMENT_3D('',#14404,#11454,#11455);
#9954=AXIS2_PLACEMENT_3D('',#14407,#11458,#11459);
#9955=AXIS2_PLACEMENT_3D('',#14408,#11460,#11461);
#9956=AXIS2_PLACEMENT_3D('',#14409,#11462,#11463);
#9957=AXIS2_PLACEMENT_3D('',#14410,#11464,#11465);
#9958=AXIS2_PLACEMENT_3D('',#14412,#11466,#11467);
#9959=AXIS2_PLACEMENT_3D('',#14415,#11469,#11470);
#9960=AXIS2_PLACEMENT_3D('',#14416,#11471,#11472);
#9961=AXIS2_PLACEMENT_3D('',#14417,#11473,#11474);
#9962=AXIS2_PLACEMENT_3D('',#14419,#11475,#11476);
#9963=AXIS2_PLACEMENT_3D('',#14422,#11478,#11479);
#9964=AXIS2_PLACEMENT_3D('',#14423,#11480,#11481);
#9965=AXIS2_PLACEMENT_3D('',#14424,#11482,#11483);
#9966=AXIS2_PLACEMENT_3D('',#14426,#11484,#11485);
#9967=AXIS2_PLACEMENT_3D('',#14429,#11487,#11488);
#9968=AXIS2_PLACEMENT_3D('',#14430,#11489,#11490);
#9969=AXIS2_PLACEMENT_3D('',#14432,#11491,#11492);
#9970=AXIS2_PLACEMENT_3D('',#14435,#11494,#11495);
#9971=AXIS2_PLACEMENT_3D('',#14436,#11496,#11497);
#9972=AXIS2_PLACEMENT_3D('',#14445,#11502,#11503);
#9973=AXIS2_PLACEMENT_3D('',#14451,#11507,#11508);
#9974=AXIS2_PLACEMENT_3D('',#14457,#11512,#11513);
#9975=AXIS2_PLACEMENT_3D('',#14460,#11516,#11517);
#9976=AXIS2_PLACEMENT_3D('',#14461,#11518,#11519);
#9977=AXIS2_PLACEMENT_3D('',#14462,#11520,#11521);
#9978=AXIS2_PLACEMENT_3D('',#14463,#11522,#11523);
#9979=AXIS2_PLACEMENT_3D('',#14465,#11524,#11525);
#9980=AXIS2_PLACEMENT_3D('',#14468,#11527,#11528);
#9981=AXIS2_PLACEMENT_3D('',#14469,#11529,#11530);
#9982=AXIS2_PLACEMENT_3D('',#14471,#11531,#11532);
#9983=AXIS2_PLACEMENT_3D('',#14474,#11534,#11535);
#9984=AXIS2_PLACEMENT_3D('',#14475,#11536,#11537);
#9985=AXIS2_PLACEMENT_3D('',#14477,#11538,#11539);
#9986=AXIS2_PLACEMENT_3D('',#14481,#11541,#11542);
#9987=AXIS2_PLACEMENT_3D('',#14485,#11544,#11545);
#9988=AXIS2_PLACEMENT_3D('',#14488,#11547,#11548);
#9989=AXIS2_PLACEMENT_3D('',#14489,#11549,#11550);
#9990=AXIS2_PLACEMENT_3D('',#14491,#11552,#11553);
#9991=AXIS2_PLACEMENT_3D('',#14493,#11554,#11555);
#9992=AXIS2_PLACEMENT_3D('',#14497,#11557,#11558);
#9993=AXIS2_PLACEMENT_3D('',#14501,#11560,#11561);
#9994=AXIS2_PLACEMENT_3D('',#14504,#11563,#11564);
#9995=AXIS2_PLACEMENT_3D('',#14505,#11565,#11566);
#9996=AXIS2_PLACEMENT_3D('',#14507,#11568,#11569);
#9997=AXIS2_PLACEMENT_3D('',#14518,#11576,#11577);
#9998=AXIS2_PLACEMENT_3D('',#14524,#11581,#11582);
#9999=AXIS2_PLACEMENT_3D('',#14530,#11586,#11587);
#10000=AXIS2_PLACEMENT_3D('',#14536,#11591,#11592);
#10001=AXIS2_PLACEMENT_3D('',#14542,#11596,#11597);
#10002=AXIS2_PLACEMENT_3D('',#14545,#11600,#11601);
#10003=AXIS2_PLACEMENT_3D('',#14546,#11602,#11603);
#10004=AXIS2_PLACEMENT_3D('',#14547,#11604,#11605);
#10005=AXIS2_PLACEMENT_3D('',#14548,#11606,#11607);
#10006=AXIS2_PLACEMENT_3D('',#14550,#11608,#11609);
#10007=AXIS2_PLACEMENT_3D('',#14553,#11611,#11612);
#10008=AXIS2_PLACEMENT_3D('',#14554,#11613,#11614);
#10009=AXIS2_PLACEMENT_3D('',#14556,#11615,#11616);
#10010=AXIS2_PLACEMENT_3D('',#14559,#11618,#11619);
#10011=AXIS2_PLACEMENT_3D('',#14560,#11620,#11621);
#10012=AXIS2_PLACEMENT_3D('',#14561,#11622,#11623);
#10013=AXIS2_PLACEMENT_3D('',#14562,#11624,#11625);
#10014=AXIS2_PLACEMENT_3D('',#15904,#11626,#11627);
#10015=AXIS2_PLACEMENT_3D('',#16040,#11628,#11629);
#10016=AXIS2_PLACEMENT_3D('',#16041,#11630,#11631);
#10017=AXIS2_PLACEMENT_3D('',#16042,#11632,#11633);
#10018=AXIS2_PLACEMENT_3D('',#16043,#11634,#11635);
#10019=AXIS2_PLACEMENT_3D('',#16044,#11636,#11637);
#10020=AXIS2_PLACEMENT_3D('',#16046,#11638,#11639);
#10021=AXIS2_PLACEMENT_3D('',#16049,#11641,#11642);
#10022=AXIS2_PLACEMENT_3D('',#16050,#11643,#11644);
#10023=AXIS2_PLACEMENT_3D('',#16051,#11645,#11646);
#10024=AXIS2_PLACEMENT_3D('',#16053,#11647,#11648);
#10025=AXIS2_PLACEMENT_3D('',#16056,#11650,#11651);
#10026=AXIS2_PLACEMENT_3D('',#16057,#11652,#11653);
#10027=AXIS2_PLACEMENT_3D('',#16058,#11654,#11655);
#10028=AXIS2_PLACEMENT_3D('',#16060,#11656,#11657);
#10029=AXIS2_PLACEMENT_3D('',#16063,#11659,#11660);
#10030=AXIS2_PLACEMENT_3D('',#16064,#11661,#11662);
#10031=AXIS2_PLACEMENT_3D('',#16066,#11663,#11664);
#10032=AXIS2_PLACEMENT_3D('',#16069,#11666,#11667);
#10033=AXIS2_PLACEMENT_3D('',#16070,#11668,#11669);
#10034=AXIS2_PLACEMENT_3D('',#16079,#11674,#11675);
#10035=AXIS2_PLACEMENT_3D('',#16085,#11679,#11680);
#10036=AXIS2_PLACEMENT_3D('',#16091,#11684,#11685);
#10037=AXIS2_PLACEMENT_3D('',#16094,#11688,#11689);
#10038=AXIS2_PLACEMENT_3D('',#16095,#11690,#11691);
#10039=AXIS2_PLACEMENT_3D('',#16096,#11692,#11693);
#10040=AXIS2_PLACEMENT_3D('',#16097,#11694,#11695);
#10041=AXIS2_PLACEMENT_3D('',#16099,#11696,#11697);
#10042=AXIS2_PLACEMENT_3D('',#16102,#11699,#11700);
#10043=AXIS2_PLACEMENT_3D('',#16103,#11701,#11702);
#10044=AXIS2_PLACEMENT_3D('',#16105,#11703,#11704);
#10045=AXIS2_PLACEMENT_3D('',#16108,#11706,#11707);
#10046=AXIS2_PLACEMENT_3D('',#16109,#11708,#11709);
#10047=AXIS2_PLACEMENT_3D('',#16111,#11710,#11711);
#10048=AXIS2_PLACEMENT_3D('',#16115,#11713,#11714);
#10049=AXIS2_PLACEMENT_3D('',#16119,#11716,#11717);
#10050=AXIS2_PLACEMENT_3D('',#16122,#11719,#11720);
#10051=AXIS2_PLACEMENT_3D('',#16123,#11721,#11722);
#10052=AXIS2_PLACEMENT_3D('',#16125,#11724,#11725);
#10053=AXIS2_PLACEMENT_3D('',#16127,#11726,#11727);
#10054=AXIS2_PLACEMENT_3D('',#16131,#11729,#11730);
#10055=AXIS2_PLACEMENT_3D('',#16135,#11732,#11733);
#10056=AXIS2_PLACEMENT_3D('',#16138,#11735,#11736);
#10057=AXIS2_PLACEMENT_3D('',#16139,#11737,#11738);
#10058=AXIS2_PLACEMENT_3D('',#16141,#11740,#11741);
#10059=AXIS2_PLACEMENT_3D('',#16152,#11748,#11749);
#10060=AXIS2_PLACEMENT_3D('',#16158,#11753,#11754);
#10061=AXIS2_PLACEMENT_3D('',#16164,#11758,#11759);
#10062=AXIS2_PLACEMENT_3D('',#16170,#11763,#11764);
#10063=AXIS2_PLACEMENT_3D('',#16176,#11768,#11769);
#10064=AXIS2_PLACEMENT_3D('',#16179,#11772,#11773);
#10065=AXIS2_PLACEMENT_3D('',#16180,#11774,#11775);
#10066=AXIS2_PLACEMENT_3D('',#16181,#11776,#11777);
#10067=AXIS2_PLACEMENT_3D('',#16182,#11778,#11779);
#10068=AXIS2_PLACEMENT_3D('',#16184,#11780,#11781);
#10069=AXIS2_PLACEMENT_3D('',#16187,#11783,#11784);
#10070=AXIS2_PLACEMENT_3D('',#16188,#11785,#11786);
#10071=AXIS2_PLACEMENT_3D('',#16190,#11787,#11788);
#10072=AXIS2_PLACEMENT_3D('',#16193,#11790,#11791);
#10073=AXIS2_PLACEMENT_3D('',#16194,#11792,#11793);
#10074=AXIS2_PLACEMENT_3D('',#16195,#11794,#11795);
#10075=AXIS2_PLACEMENT_3D('',#16196,#11796,#11797);
#10076=AXIS2_PLACEMENT_3D('',#17468,#11798,#11799);
#10077=AXIS2_PLACEMENT_3D('',#17597,#11800,#11801);
#10078=AXIS2_PLACEMENT_3D('',#17598,#11802,#11803);
#10079=AXIS2_PLACEMENT_3D('',#17599,#11804,#11805);
#10080=AXIS2_PLACEMENT_3D('',#17600,#11806,#11807);
#10081=AXIS2_PLACEMENT_3D('',#17601,#11808,#11809);
#10082=AXIS2_PLACEMENT_3D('',#17603,#11810,#11811);
#10083=AXIS2_PLACEMENT_3D('',#17606,#11813,#11814);
#10084=AXIS2_PLACEMENT_3D('',#17607,#11815,#11816);
#10085=AXIS2_PLACEMENT_3D('',#17608,#11817,#11818);
#10086=AXIS2_PLACEMENT_3D('',#17610,#11819,#11820);
#10087=AXIS2_PLACEMENT_3D('',#17613,#11822,#11823);
#10088=AXIS2_PLACEMENT_3D('',#17614,#11824,#11825);
#10089=AXIS2_PLACEMENT_3D('',#17615,#11826,#11827);
#10090=AXIS2_PLACEMENT_3D('',#17617,#11828,#11829);
#10091=AXIS2_PLACEMENT_3D('',#17620,#11831,#11832);
#10092=AXIS2_PLACEMENT_3D('',#17621,#11833,#11834);
#10093=AXIS2_PLACEMENT_3D('',#17623,#11835,#11836);
#10094=AXIS2_PLACEMENT_3D('',#17626,#11838,#11839);
#10095=AXIS2_PLACEMENT_3D('',#17627,#11840,#11841);
#10096=AXIS2_PLACEMENT_3D('',#17636,#11846,#11847);
#10097=AXIS2_PLACEMENT_3D('',#17642,#11851,#11852);
#10098=AXIS2_PLACEMENT_3D('',#17648,#11856,#11857);
#10099=AXIS2_PLACEMENT_3D('',#17651,#11860,#11861);
#10100=AXIS2_PLACEMENT_3D('',#17652,#11862,#11863);
#10101=AXIS2_PLACEMENT_3D('',#17653,#11864,#11865);
#10102=AXIS2_PLACEMENT_3D('',#17654,#11866,#11867);
#10103=AXIS2_PLACEMENT_3D('',#17656,#11868,#11869);
#10104=AXIS2_PLACEMENT_3D('',#17659,#11871,#11872);
#10105=AXIS2_PLACEMENT_3D('',#17660,#11873,#11874);
#10106=AXIS2_PLACEMENT_3D('',#17662,#11875,#11876);
#10107=AXIS2_PLACEMENT_3D('',#17665,#11878,#11879);
#10108=AXIS2_PLACEMENT_3D('',#17666,#11880,#11881);
#10109=AXIS2_PLACEMENT_3D('',#17668,#11882,#11883);
#10110=AXIS2_PLACEMENT_3D('',#17672,#11885,#11886);
#10111=AXIS2_PLACEMENT_3D('',#17676,#11888,#11889);
#10112=AXIS2_PLACEMENT_3D('',#17679,#11891,#11892);
#10113=AXIS2_PLACEMENT_3D('',#17680,#11893,#11894);
#10114=AXIS2_PLACEMENT_3D('',#17682,#11896,#11897);
#10115=AXIS2_PLACEMENT_3D('',#17684,#11898,#11899);
#10116=AXIS2_PLACEMENT_3D('',#17688,#11901,#11902);
#10117=AXIS2_PLACEMENT_3D('',#17692,#11904,#11905);
#10118=AXIS2_PLACEMENT_3D('',#17695,#11907,#11908);
#10119=AXIS2_PLACEMENT_3D('',#17696,#11909,#11910);
#10120=AXIS2_PLACEMENT_3D('',#17698,#11912,#11913);
#10121=AXIS2_PLACEMENT_3D('',#17709,#11920,#11921);
#10122=AXIS2_PLACEMENT_3D('',#17715,#11925,#11926);
#10123=AXIS2_PLACEMENT_3D('',#17721,#11930,#11931);
#10124=AXIS2_PLACEMENT_3D('',#17727,#11935,#11936);
#10125=AXIS2_PLACEMENT_3D('',#17733,#11940,#11941);
#10126=AXIS2_PLACEMENT_3D('',#17736,#11944,#11945);
#10127=AXIS2_PLACEMENT_3D('',#17737,#11946,#11947);
#10128=AXIS2_PLACEMENT_3D('',#17738,#11948,#11949);
#10129=AXIS2_PLACEMENT_3D('',#17739,#11950,#11951);
#10130=AXIS2_PLACEMENT_3D('',#17741,#11952,#11953);
#10131=AXIS2_PLACEMENT_3D('',#17744,#11955,#11956);
#10132=AXIS2_PLACEMENT_3D('',#17745,#11957,#11958);
#10133=AXIS2_PLACEMENT_3D('',#17747,#11959,#11960);
#10134=AXIS2_PLACEMENT_3D('',#17750,#11962,#11963);
#10135=AXIS2_PLACEMENT_3D('',#17751,#11964,#11965);
#10136=AXIS2_PLACEMENT_3D('',#17752,#11966,#11967);
#10137=AXIS2_PLACEMENT_3D('',#17753,#11968,#11969);
#10138=AXIS2_PLACEMENT_3D('',#19135,#11970,#11971);
#10139=AXIS2_PLACEMENT_3D('',#19275,#11972,#11973);
#10140=AXIS2_PLACEMENT_3D('',#19276,#11974,#11975);
#10141=AXIS2_PLACEMENT_3D('',#19277,#11976,#11977);
#10142=AXIS2_PLACEMENT_3D('',#19278,#11978,#11979);
#10143=AXIS2_PLACEMENT_3D('',#19279,#11980,#11981);
#10144=AXIS2_PLACEMENT_3D('',#19281,#11982,#11983);
#10145=AXIS2_PLACEMENT_3D('',#19284,#11985,#11986);
#10146=AXIS2_PLACEMENT_3D('',#19285,#11987,#11988);
#10147=AXIS2_PLACEMENT_3D('',#19286,#11989,#11990);
#10148=AXIS2_PLACEMENT_3D('',#19288,#11991,#11992);
#10149=AXIS2_PLACEMENT_3D('',#19291,#11994,#11995);
#10150=AXIS2_PLACEMENT_3D('',#19292,#11996,#11997);
#10151=AXIS2_PLACEMENT_3D('',#19293,#11998,#11999);
#10152=AXIS2_PLACEMENT_3D('',#19295,#12000,#12001);
#10153=AXIS2_PLACEMENT_3D('',#19298,#12003,#12004);
#10154=AXIS2_PLACEMENT_3D('',#19299,#12005,#12006);
#10155=AXIS2_PLACEMENT_3D('',#19301,#12007,#12008);
#10156=AXIS2_PLACEMENT_3D('',#19304,#12010,#12011);
#10157=AXIS2_PLACEMENT_3D('',#19305,#12012,#12013);
#10158=AXIS2_PLACEMENT_3D('',#19314,#12018,#12019);
#10159=AXIS2_PLACEMENT_3D('',#19320,#12023,#12024);
#10160=AXIS2_PLACEMENT_3D('',#19326,#12028,#12029);
#10161=AXIS2_PLACEMENT_3D('',#19329,#12032,#12033);
#10162=AXIS2_PLACEMENT_3D('',#19330,#12034,#12035);
#10163=AXIS2_PLACEMENT_3D('',#19331,#12036,#12037);
#10164=AXIS2_PLACEMENT_3D('',#19332,#12038,#12039);
#10165=AXIS2_PLACEMENT_3D('',#19334,#12040,#12041);
#10166=AXIS2_PLACEMENT_3D('',#19337,#12043,#12044);
#10167=AXIS2_PLACEMENT_3D('',#19338,#12045,#12046);
#10168=AXIS2_PLACEMENT_3D('',#19340,#12047,#12048);
#10169=AXIS2_PLACEMENT_3D('',#19343,#12050,#12051);
#10170=AXIS2_PLACEMENT_3D('',#19344,#12052,#12053);
#10171=AXIS2_PLACEMENT_3D('',#19346,#12054,#12055);
#10172=AXIS2_PLACEMENT_3D('',#19350,#12057,#12058);
#10173=AXIS2_PLACEMENT_3D('',#19354,#12060,#12061);
#10174=AXIS2_PLACEMENT_3D('',#19357,#12063,#12064);
#10175=AXIS2_PLACEMENT_3D('',#19358,#12065,#12066);
#10176=AXIS2_PLACEMENT_3D('',#19360,#12068,#12069);
#10177=AXIS2_PLACEMENT_3D('',#19362,#12070,#12071);
#10178=AXIS2_PLACEMENT_3D('',#19366,#12073,#12074);
#10179=AXIS2_PLACEMENT_3D('',#19370,#12076,#12077);
#10180=AXIS2_PLACEMENT_3D('',#19373,#12079,#12080);
#10181=AXIS2_PLACEMENT_3D('',#19374,#12081,#12082);
#10182=AXIS2_PLACEMENT_3D('',#19376,#12084,#12085);
#10183=AXIS2_PLACEMENT_3D('',#19387,#12092,#12093);
#10184=AXIS2_PLACEMENT_3D('',#19393,#12097,#12098);
#10185=AXIS2_PLACEMENT_3D('',#19399,#12102,#12103);
#10186=AXIS2_PLACEMENT_3D('',#19405,#12107,#12108);
#10187=AXIS2_PLACEMENT_3D('',#19411,#12112,#12113);
#10188=AXIS2_PLACEMENT_3D('',#19414,#12116,#12117);
#10189=AXIS2_PLACEMENT_3D('',#19415,#12118,#12119);
#10190=AXIS2_PLACEMENT_3D('',#19416,#12120,#12121);
#10191=AXIS2_PLACEMENT_3D('',#19417,#12122,#12123);
#10192=AXIS2_PLACEMENT_3D('',#19419,#12124,#12125);
#10193=AXIS2_PLACEMENT_3D('',#19422,#12127,#12128);
#10194=AXIS2_PLACEMENT_3D('',#19423,#12129,#12130);
#10195=AXIS2_PLACEMENT_3D('',#19425,#12131,#12132);
#10196=AXIS2_PLACEMENT_3D('',#19428,#12134,#12135);
#10197=AXIS2_PLACEMENT_3D('',#19429,#12136,#12137);
#10198=AXIS2_PLACEMENT_3D('',#19430,#12138,#12139);
#10199=AXIS2_PLACEMENT_3D('',#19431,#12140,#12141);
#10200=AXIS2_PLACEMENT_3D('',#20703,#12142,#12143);
#10201=AXIS2_PLACEMENT_3D('',#20832,#12144,#12145);
#10202=AXIS2_PLACEMENT_3D('',#20833,#12146,#12147);
#10203=AXIS2_PLACEMENT_3D('',#20834,#12148,#12149);
#10204=AXIS2_PLACEMENT_3D('',#20835,#12150,#12151);
#10205=AXIS2_PLACEMENT_3D('',#20836,#12152,#12153);
#10206=AXIS2_PLACEMENT_3D('',#20838,#12154,#12155);
#10207=AXIS2_PLACEMENT_3D('',#20841,#12157,#12158);
#10208=AXIS2_PLACEMENT_3D('',#20842,#12159,#12160);
#10209=AXIS2_PLACEMENT_3D('',#20843,#12161,#12162);
#10210=AXIS2_PLACEMENT_3D('',#20845,#12163,#12164);
#10211=AXIS2_PLACEMENT_3D('',#20848,#12166,#12167);
#10212=AXIS2_PLACEMENT_3D('',#20849,#12168,#12169);
#10213=AXIS2_PLACEMENT_3D('',#20850,#12170,#12171);
#10214=AXIS2_PLACEMENT_3D('',#20852,#12172,#12173);
#10215=AXIS2_PLACEMENT_3D('',#20855,#12175,#12176);
#10216=AXIS2_PLACEMENT_3D('',#20856,#12177,#12178);
#10217=AXIS2_PLACEMENT_3D('',#20857,#12179,#12180);
#10218=AXIS2_PLACEMENT_3D('',#20859,#12181,#12182);
#10219=AXIS2_PLACEMENT_3D('',#20862,#12184,#12185);
#10220=AXIS2_PLACEMENT_3D('',#20863,#12186,#12187);
#10221=AXIS2_PLACEMENT_3D('',#20864,#12188,#12189);
#10222=AXIS2_PLACEMENT_3D('',#20866,#12190,#12191);
#10223=AXIS2_PLACEMENT_3D('',#20869,#12193,#12194);
#10224=AXIS2_PLACEMENT_3D('',#20870,#12195,#12196);
#10225=AXIS2_PLACEMENT_3D('',#20871,#12197,#12198);
#10226=AXIS2_PLACEMENT_3D('',#20873,#12199,#12200);
#10227=AXIS2_PLACEMENT_3D('',#20876,#12202,#12203);
#10228=AXIS2_PLACEMENT_3D('',#20877,#12204,#12205);
#10229=AXIS2_PLACEMENT_3D('',#20878,#12206,#12207);
#10230=AXIS2_PLACEMENT_3D('',#20887,#12212,#12213);
#10231=AXIS2_PLACEMENT_3D('',#20893,#12217,#12218);
#10232=AXIS2_PLACEMENT_3D('',#20899,#12222,#12223);
#10233=AXIS2_PLACEMENT_3D('',#20902,#12226,#12227);
#10234=AXIS2_PLACEMENT_3D('',#20903,#12228,#12229);
#10235=AXIS2_PLACEMENT_3D('',#20904,#12230,#12231);
#10236=AXIS2_PLACEMENT_3D('',#20905,#12232,#12233);
#10237=AXIS2_PLACEMENT_3D('',#20907,#12234,#12235);
#10238=AXIS2_PLACEMENT_3D('',#20910,#12237,#12238);
#10239=AXIS2_PLACEMENT_3D('',#20911,#12239,#12240);
#10240=AXIS2_PLACEMENT_3D('',#20913,#12241,#12242);
#10241=AXIS2_PLACEMENT_3D('',#20916,#12244,#12245);
#10242=AXIS2_PLACEMENT_3D('',#20917,#12246,#12247);
#10243=AXIS2_PLACEMENT_3D('',#20919,#12248,#12249);
#10244=AXIS2_PLACEMENT_3D('',#20922,#12251,#12252);
#10245=AXIS2_PLACEMENT_3D('',#20923,#12253,#12254);
#10246=AXIS2_PLACEMENT_3D('',#20925,#12255,#12256);
#10247=AXIS2_PLACEMENT_3D('',#20928,#12258,#12259);
#10248=AXIS2_PLACEMENT_3D('',#20929,#12260,#12261);
#10249=AXIS2_PLACEMENT_3D('',#20931,#12262,#12263);
#10250=AXIS2_PLACEMENT_3D('',#20934,#12265,#12266);
#10251=AXIS2_PLACEMENT_3D('',#20935,#12267,#12268);
#10252=AXIS2_PLACEMENT_3D('',#20937,#12269,#12270);
#10253=AXIS2_PLACEMENT_3D('',#20940,#12272,#12273);
#10254=AXIS2_PLACEMENT_3D('',#20941,#12274,#12275);
#10255=AXIS2_PLACEMENT_3D('',#20943,#12276,#12277);
#10256=AXIS2_PLACEMENT_3D('',#20946,#12279,#12280);
#10257=AXIS2_PLACEMENT_3D('',#20947,#12281,#12282);
#10258=AXIS2_PLACEMENT_3D('',#20949,#12283,#12284);
#10259=AXIS2_PLACEMENT_3D('',#20952,#12286,#12287);
#10260=AXIS2_PLACEMENT_3D('',#20953,#12288,#12289);
#10261=AXIS2_PLACEMENT_3D('',#20962,#12294,#12295);
#10262=AXIS2_PLACEMENT_3D('',#20968,#12299,#12300);
#10263=AXIS2_PLACEMENT_3D('',#20974,#12304,#12305);
#10264=AXIS2_PLACEMENT_3D('',#20977,#12308,#12309);
#10265=AXIS2_PLACEMENT_3D('',#20978,#12310,#12311);
#10266=AXIS2_PLACEMENT_3D('',#20979,#12312,#12313);
#10267=AXIS2_PLACEMENT_3D('',#20980,#12314,#12315);
#10268=AXIS2_PLACEMENT_3D('',#20982,#12316,#12317);
#10269=AXIS2_PLACEMENT_3D('',#20985,#12319,#12320);
#10270=AXIS2_PLACEMENT_3D('',#20986,#12321,#12322);
#10271=AXIS2_PLACEMENT_3D('',#20988,#12323,#12324);
#10272=AXIS2_PLACEMENT_3D('',#20991,#12326,#12327);
#10273=AXIS2_PLACEMENT_3D('',#20992,#12328,#12329);
#10274=AXIS2_PLACEMENT_3D('',#20993,#12330,#12331);
#10275=AXIS2_PLACEMENT_3D('',#20994,#12332,#12333);
#10276=AXIS2_PLACEMENT_3D('',#20995,#12334,#12335);
#10277=AXIS2_PLACEMENT_3D('',#20997,#12336,#12337);
#10278=AXIS2_PLACEMENT_3D('',#21000,#12339,#12340);
#10279=AXIS2_PLACEMENT_3D('',#21001,#12341,#12342);
#10280=AXIS2_PLACEMENT_3D('',#21002,#12343,#12344);
#10281=AXIS2_PLACEMENT_3D('',#21004,#12345,#12346);
#10282=AXIS2_PLACEMENT_3D('',#21007,#12348,#12349);
#10283=AXIS2_PLACEMENT_3D('',#21008,#12350,#12351);
#10284=AXIS2_PLACEMENT_3D('',#21009,#12352,#12353);
#10285=AXIS2_PLACEMENT_3D('',#21010,#12354,#12355);
#10286=AXIS2_PLACEMENT_3D('',#21011,#12356,#12357);
#10287=AXIS2_PLACEMENT_3D('',#21013,#12358,#12359);
#10288=AXIS2_PLACEMENT_3D('',#21016,#12361,#12362);
#10289=AXIS2_PLACEMENT_3D('',#21017,#12363,#12364);
#10290=AXIS2_PLACEMENT_3D('',#21018,#12365,#12366);
#10291=AXIS2_PLACEMENT_3D('',#21019,#12367,#12368);
#10292=AXIS2_PLACEMENT_3D('',#21020,#12369,#12370);
#10293=AXIS2_PLACEMENT_3D('',#21022,#12371,#12372);
#10294=AXIS2_PLACEMENT_3D('',#21025,#12374,#12375);
#10295=AXIS2_PLACEMENT_3D('',#21026,#12376,#12377);
#10296=AXIS2_PLACEMENT_3D('',#21027,#12378,#12379);
#10297=AXIS2_PLACEMENT_3D('',#21029,#12380,#12381);
#10298=AXIS2_PLACEMENT_3D('',#21032,#12383,#12384);
#10299=AXIS2_PLACEMENT_3D('',#21033,#12385,#12386);
#10300=AXIS2_PLACEMENT_3D('',#21034,#12387,#12388);
#10301=AXIS2_PLACEMENT_3D('',#21035,#12389,#12390);
#10302=AXIS2_PLACEMENT_3D('',#21036,#12391,#12392);
#10303=AXIS2_PLACEMENT_3D('',#21038,#12393,#12394);
#10304=AXIS2_PLACEMENT_3D('',#21041,#12396,#12397);
#10305=AXIS2_PLACEMENT_3D('',#21042,#12398,#12399);
#10306=AXIS2_PLACEMENT_3D('',#21043,#12400,#12401);
#10307=AXIS2_PLACEMENT_3D('',#21044,#12402,#12403);
#10308=AXIS2_PLACEMENT_3D('',#21045,#12404,#12405);
#10309=AXIS2_PLACEMENT_3D('',#21047,#12406,#12407);
#10310=AXIS2_PLACEMENT_3D('',#21050,#12409,#12410);
#10311=AXIS2_PLACEMENT_3D('',#21051,#12411,#12412);
#10312=AXIS2_PLACEMENT_3D('',#21052,#12413,#12414);
#10313=AXIS2_PLACEMENT_3D('',#21054,#12415,#12416);
#10314=AXIS2_PLACEMENT_3D('',#21057,#12418,#12419);
#10315=AXIS2_PLACEMENT_3D('',#21058,#12420,#12421);
#10316=AXIS2_PLACEMENT_3D('',#21059,#12422,#12423);
#10317=AXIS2_PLACEMENT_3D('',#21060,#12424,#12425);
#10318=AXIS2_PLACEMENT_3D('',#21061,#12426,#12427);
#10319=AXIS2_PLACEMENT_3D('',#21063,#12428,#12429);
#10320=AXIS2_PLACEMENT_3D('',#21066,#12431,#12432);
#10321=AXIS2_PLACEMENT_3D('',#21067,#12433,#12434);
#10322=AXIS2_PLACEMENT_3D('',#21068,#12435,#12436);
#10323=AXIS2_PLACEMENT_3D('',#21069,#12437,#12438);
#10324=AXIS2_PLACEMENT_3D('',#21070,#12439,#12440);
#10325=AXIS2_PLACEMENT_3D('',#21072,#12441,#12442);
#10326=AXIS2_PLACEMENT_3D('',#21075,#12444,#12445);
#10327=AXIS2_PLACEMENT_3D('',#21076,#12446,#12447);
#10328=AXIS2_PLACEMENT_3D('',#21077,#12448,#12449);
#10329=AXIS2_PLACEMENT_3D('',#21079,#12450,#12451);
#10330=AXIS2_PLACEMENT_3D('',#21082,#12453,#12454);
#10331=AXIS2_PLACEMENT_3D('',#21083,#12455,#12456);
#10332=AXIS2_PLACEMENT_3D('',#21084,#12457,#12458);
#10333=AXIS2_PLACEMENT_3D('',#21085,#12459,#12460);
#10334=AXIS2_PLACEMENT_3D('',#21086,#12461,#12462);
#10335=AXIS2_PLACEMENT_3D('',#21088,#12463,#12464);
#10336=AXIS2_PLACEMENT_3D('',#21091,#12466,#12467);
#10337=AXIS2_PLACEMENT_3D('',#21092,#12468,#12469);
#10338=AXIS2_PLACEMENT_3D('',#21093,#12470,#12471);
#10339=AXIS2_PLACEMENT_3D('',#21094,#12472,#12473);
#10340=AXIS2_PLACEMENT_3D('',#21095,#12474,#12475);
#10341=AXIS2_PLACEMENT_3D('',#21097,#12476,#12477);
#10342=AXIS2_PLACEMENT_3D('',#21100,#12479,#12480);
#10343=AXIS2_PLACEMENT_3D('',#21101,#12481,#12482);
#10344=AXIS2_PLACEMENT_3D('',#21103,#12483,#12484);
#10345=AXIS2_PLACEMENT_3D('',#21105,#12486,#12487);
#10346=AXIS2_PLACEMENT_3D('',#21106,#12488,#12489);
#10347=AXIS2_PLACEMENT_3D('',#21108,#12490,#12491);
#10348=AXIS2_PLACEMENT_3D('',#21110,#12493,#12494);
#10349=AXIS2_PLACEMENT_3D('',#21111,#12495,#12496);
#10350=AXIS2_PLACEMENT_3D('',#21112,#12497,#12498);
#10351=AXIS2_PLACEMENT_3D('',#21116,#12500,#12501);
#10352=AXIS2_PLACEMENT_3D('',#21117,#12502,#12503);
#10353=AXIS2_PLACEMENT_3D('',#21121,#12505,#12506);
#10354=AXIS2_PLACEMENT_3D('',#21123,#12508,#12509);
#10355=AXIS2_PLACEMENT_3D('',#21128,#12511,#12512);
#10356=AXIS2_PLACEMENT_3D('',#21131,#12514,#12515);
#10357=AXIS2_PLACEMENT_3D('',#21132,#12516,#12517);
#10358=AXIS2_PLACEMENT_3D('',#21134,#12519,#12520);
#10359=AXIS2_PLACEMENT_3D('',#21145,#12526,#12527);
#10360=AXIS2_PLACEMENT_3D('',#21146,#12528,#12529);
#10361=AXIS2_PLACEMENT_3D('',#21153,#12533,#12534);
#10362=AXIS2_PLACEMENT_3D('',#21154,#12535,#12536);
#10363=AXIS2_PLACEMENT_3D('',#21165,#12542,#12543);
#10364=AXIS2_PLACEMENT_3D('',#21166,#12544,#12545);
#10365=AXIS2_PLACEMENT_3D('',#21168,#12546,#12547);
#10366=AXIS2_PLACEMENT_3D('',#21171,#12549,#12550);
#10367=AXIS2_PLACEMENT_3D('',#21172,#12551,#12552);
#10368=AXIS2_PLACEMENT_3D('',#21175,#12554,#12555);
#10369=AXIS2_PLACEMENT_3D('',#21176,#12556,#12557);
#10370=AXIS2_PLACEMENT_3D('',#21178,#12558,#12559);
#10371=AXIS2_PLACEMENT_3D('',#21180,#12561,#12562);
#10372=AXIS2_PLACEMENT_3D('',#21182,#12563,#12564);
#10373=AXIS2_PLACEMENT_3D('',#21184,#12566,#12567);
#10374=AXIS2_PLACEMENT_3D('',#21186,#12568,#12569);
#10375=AXIS2_PLACEMENT_3D('',#21189,#12571,#12572);
#10376=AXIS2_PLACEMENT_3D('',#21190,#12573,#12574);
#10377=AXIS2_PLACEMENT_3D('',#21207,#12584,#12585);
#10378=AXIS2_PLACEMENT_3D('',#21211,#12588,#12589);
#10379=AXIS2_PLACEMENT_3D('',#21215,#12592,#12593);
#10380=AXIS2_PLACEMENT_3D('',#21217,#12595,#12596);
#10381=AXIS2_PLACEMENT_3D('',#21221,#12599,#12600);
#10382=AXIS2_PLACEMENT_3D('',#21225,#12603,#12604);
#10383=AXIS2_PLACEMENT_3D('',#21229,#12607,#12608);
#10384=AXIS2_PLACEMENT_3D('',#21233,#12611,#12612);
#10385=AXIS2_PLACEMENT_3D('',#21237,#12615,#12616);
#10386=AXIS2_PLACEMENT_3D('',#21239,#12618,#12619);
#10387=AXIS2_PLACEMENT_3D('',#21240,#12620,#12621);
#10388=AXIS2_PLACEMENT_3D('',#21241,#12622,#12623);
#10389=AXIS2_PLACEMENT_3D('',#21250,#12628,#12629);
#10390=AXIS2_PLACEMENT_3D('',#21256,#12633,#12634);
#10391=AXIS2_PLACEMENT_3D('',#21262,#12638,#12639);
#10392=AXIS2_PLACEMENT_3D('',#21268,#12643,#12644);
#10393=AXIS2_PLACEMENT_3D('',#21274,#12648,#12649);
#10394=AXIS2_PLACEMENT_3D('',#21277,#12652,#12653);
#10395=AXIS2_PLACEMENT_3D('',#21278,#12654,#12655);
#10396=AXIS2_PLACEMENT_3D('',#21279,#12656,#12657);
#10397=AXIS2_PLACEMENT_3D('',#21281,#12658,#12659);
#10398=AXIS2_PLACEMENT_3D('',#21282,#12660,#12661);
#10399=AXIS2_PLACEMENT_3D('',#21284,#12662,#12663);
#10400=AXIS2_PLACEMENT_3D('',#21285,#12664,#12665);
#10401=AXIS2_PLACEMENT_3D('',#21287,#12666,#12667);
#10402=AXIS2_PLACEMENT_3D('',#21289,#12669,#12670);
#10403=AXIS2_PLACEMENT_3D('',#21291,#12671,#12672);
#10404=AXIS2_PLACEMENT_3D('',#21293,#12674,#12675);
#10405=AXIS2_PLACEMENT_3D('',#21295,#12676,#12677);
#10406=AXIS2_PLACEMENT_3D('',#21297,#12679,#12680);
#10407=AXIS2_PLACEMENT_3D('',#21299,#12681,#12682);
#10408=AXIS2_PLACEMENT_3D('',#21300,#12683,#12684);
#10409=AXIS2_PLACEMENT_3D('',#21302,#12685,#12686);
#10410=AXIS2_PLACEMENT_3D('',#21304,#12688,#12689);
#10411=AXIS2_PLACEMENT_3D('',#21306,#12691,#12692);
#10412=AXIS2_PLACEMENT_3D('',#21307,#12693,#12694);
#10413=AXIS2_PLACEMENT_3D('',#21309,#12695,#12696);
#10414=AXIS2_PLACEMENT_3D('',#21310,#12697,#12698);
#10415=AXIS2_PLACEMENT_3D('',#21312,#12699,#12700);
#10416=AXIS2_PLACEMENT_3D('',#21314,#12702,#12703);
#10417=AXIS2_PLACEMENT_3D('',#21316,#12704,#12705);
#10418=AXIS2_PLACEMENT_3D('',#21318,#12707,#12708);
#10419=AXIS2_PLACEMENT_3D('',#21320,#12709,#12710);
#10420=AXIS2_PLACEMENT_3D('',#21322,#12712,#12713);
#10421=AXIS2_PLACEMENT_3D('',#21324,#12714,#12715);
#10422=AXIS2_PLACEMENT_3D('',#21325,#12716,#12717);
#10423=AXIS2_PLACEMENT_3D('',#21327,#12718,#12719);
#10424=AXIS2_PLACEMENT_3D('',#21329,#12721,#12722);
#10425=AXIS2_PLACEMENT_3D('',#21331,#12723,#12724);
#10426=AXIS2_PLACEMENT_3D('',#21333,#12726,#12727);
#10427=AXIS2_PLACEMENT_3D('',#21335,#12728,#12729);
#10428=AXIS2_PLACEMENT_3D('',#21337,#12731,#12732);
#10429=AXIS2_PLACEMENT_3D('',#21338,#12733,#12734);
#10430=AXIS2_PLACEMENT_3D('',#21347,#12739,#12740);
#10431=AXIS2_PLACEMENT_3D('',#21353,#12744,#12745);
#10432=AXIS2_PLACEMENT_3D('',#21359,#12749,#12750);
#10433=AXIS2_PLACEMENT_3D('',#21365,#12754,#12755);
#10434=AXIS2_PLACEMENT_3D('',#21371,#12759,#12760);
#10435=AXIS2_PLACEMENT_3D('',#21374,#12763,#12764);
#10436=AXIS2_PLACEMENT_3D('',#21375,#12765,#12766);
#10437=AXIS2_PLACEMENT_3D('',#21376,#12767,#12768);
#10438=AXIS2_PLACEMENT_3D('',#21377,#12769,#12770);
#10439=AXIS2_PLACEMENT_3D('',#21378,#12771,#12772);
#10440=AXIS2_PLACEMENT_3D('',#21380,#12773,#12774);
#10441=AXIS2_PLACEMENT_3D('',#21383,#12776,#12777);
#10442=AXIS2_PLACEMENT_3D('',#21384,#12778,#12779);
#10443=AXIS2_PLACEMENT_3D('',#21386,#12780,#12781);
#10444=AXIS2_PLACEMENT_3D('',#21389,#12783,#12784);
#10445=AXIS2_PLACEMENT_3D('',#21390,#12785,#12786);
#10446=AXIS2_PLACEMENT_3D('',#21392,#12787,#12788);
#10447=AXIS2_PLACEMENT_3D('',#21395,#12790,#12791);
#10448=AXIS2_PLACEMENT_3D('',#21396,#12792,#12793);
#10449=AXIS2_PLACEMENT_3D('',#21398,#12794,#12795);
#10450=AXIS2_PLACEMENT_3D('',#21401,#12797,#12798);
#10451=AXIS2_PLACEMENT_3D('',#21402,#12799,#12800);
#10452=AXIS2_PLACEMENT_3D('',#21404,#12801,#12802);
#10453=AXIS2_PLACEMENT_3D('',#21407,#12804,#12805);
#10454=AXIS2_PLACEMENT_3D('',#21408,#12806,#12807);
#10455=AXIS2_PLACEMENT_3D('',#21410,#12808,#12809);
#10456=AXIS2_PLACEMENT_3D('',#21413,#12811,#12812);
#10457=AXIS2_PLACEMENT_3D('',#21414,#12813,#12814);
#10458=AXIS2_PLACEMENT_3D('',#21416,#12815,#12816);
#10459=AXIS2_PLACEMENT_3D('',#21419,#12818,#12819);
#10460=AXIS2_PLACEMENT_3D('',#21420,#12820,#12821);
#10461=AXIS2_PLACEMENT_3D('',#21422,#12822,#12823);
#10462=AXIS2_PLACEMENT_3D('',#21425,#12825,#12826);
#10463=AXIS2_PLACEMENT_3D('',#21426,#12827,#12828);
#10464=AXIS2_PLACEMENT_3D('',#21428,#12829,#12830);
#10465=AXIS2_PLACEMENT_3D('',#21431,#12832,#12833);
#10466=AXIS2_PLACEMENT_3D('',#21432,#12834,#12835);
#10467=AXIS2_PLACEMENT_3D('',#21434,#12836,#12837);
#10468=AXIS2_PLACEMENT_3D('',#21437,#12839,#12840);
#10469=AXIS2_PLACEMENT_3D('',#21438,#12841,#12842);
#10470=AXIS2_PLACEMENT_3D('',#21440,#12843,#12844);
#10471=AXIS2_PLACEMENT_3D('',#21443,#12846,#12847);
#10472=AXIS2_PLACEMENT_3D('',#21444,#12848,#12849);
#10473=AXIS2_PLACEMENT_3D('',#21446,#12850,#12851);
#10474=AXIS2_PLACEMENT_3D('',#21449,#12853,#12854);
#10475=AXIS2_PLACEMENT_3D('',#21450,#12855,#12856);
#10476=AXIS2_PLACEMENT_3D('',#21452,#12857,#12858);
#10477=AXIS2_PLACEMENT_3D('',#21455,#12860,#12861);
#10478=AXIS2_PLACEMENT_3D('',#21456,#12862,#12863);
#10479=AXIS2_PLACEMENT_3D('',#21458,#12864,#12865);
#10480=AXIS2_PLACEMENT_3D('',#21461,#12867,#12868);
#10481=AXIS2_PLACEMENT_3D('',#21462,#12869,#12870);
#10482=AXIS2_PLACEMENT_3D('',#21464,#12871,#12872);
#10483=AXIS2_PLACEMENT_3D('',#21467,#12874,#12875);
#10484=AXIS2_PLACEMENT_3D('',#21468,#12876,#12877);
#10485=AXIS2_PLACEMENT_3D('',#21470,#12878,#12879);
#10486=AXIS2_PLACEMENT_3D('',#21473,#12881,#12882);
#10487=AXIS2_PLACEMENT_3D('',#21474,#12883,#12884);
#10488=AXIS2_PLACEMENT_3D('',#21476,#12885,#12886);
#10489=AXIS2_PLACEMENT_3D('',#21479,#12888,#12889);
#10490=AXIS2_PLACEMENT_3D('',#21480,#12890,#12891);
#10491=AXIS2_PLACEMENT_3D('',#21482,#12892,#12893);
#10492=AXIS2_PLACEMENT_3D('',#21485,#12895,#12896);
#10493=AXIS2_PLACEMENT_3D('',#21486,#12897,#12898);
#10494=AXIS2_PLACEMENT_3D('',#21488,#12899,#12900);
#10495=AXIS2_PLACEMENT_3D('',#21491,#12902,#12903);
#10496=AXIS2_PLACEMENT_3D('',#21492,#12904,#12905);
#10497=AXIS2_PLACEMENT_3D('',#21494,#12906,#12907);
#10498=AXIS2_PLACEMENT_3D('',#21497,#12909,#12910);
#10499=AXIS2_PLACEMENT_3D('',#21498,#12911,#12912);
#10500=AXIS2_PLACEMENT_3D('',#21500,#12913,#12914);
#10501=AXIS2_PLACEMENT_3D('',#21503,#12916,#12917);
#10502=AXIS2_PLACEMENT_3D('',#21504,#12918,#12919);
#10503=AXIS2_PLACEMENT_3D('',#21506,#12920,#12921);
#10504=AXIS2_PLACEMENT_3D('',#21509,#12923,#12924);
#10505=AXIS2_PLACEMENT_3D('',#21510,#12925,#12926);
#10506=AXIS2_PLACEMENT_3D('',#21512,#12927,#12928);
#10507=AXIS2_PLACEMENT_3D('',#21515,#12930,#12931);
#10508=AXIS2_PLACEMENT_3D('',#21516,#12932,#12933);
#10509=AXIS2_PLACEMENT_3D('',#21518,#12934,#12935);
#10510=AXIS2_PLACEMENT_3D('',#21521,#12937,#12938);
#10511=AXIS2_PLACEMENT_3D('',#21522,#12939,#12940);
#10512=AXIS2_PLACEMENT_3D('',#21531,#12945,#12946);
#10513=AXIS2_PLACEMENT_3D('',#21537,#12950,#12951);
#10514=AXIS2_PLACEMENT_3D('',#21543,#12955,#12956);
#10515=AXIS2_PLACEMENT_3D('',#21546,#12959,#12960);
#10516=AXIS2_PLACEMENT_3D('',#21547,#12961,#12962);
#10517=AXIS2_PLACEMENT_3D('',#21548,#12963,#12964);
#10518=AXIS2_PLACEMENT_3D('',#21549,#12965,#12966);
#10519=AXIS2_PLACEMENT_3D('',#21552,#12967,#12968);
#10520=AXIS2_PLACEMENT_3D('',#21553,#12969,#12970);
#10521=AXIS2_PLACEMENT_3D('',#21554,#12971,#12972);
#10522=AXIS2_PLACEMENT_3D('',#21558,#12974,#12975);
#10523=AXIS2_PLACEMENT_3D('',#21561,#12977,#12978);
#10524=AXIS2_PLACEMENT_3D('',#21563,#12979,#12980);
#10525=AXIS2_PLACEMENT_3D('',#21565,#12982,#12983);
#10526=AXIS2_PLACEMENT_3D('',#21568,#12984,#12985);
#10527=AXIS2_PLACEMENT_3D('',#21569,#12986,#12987);
#10528=AXIS2_PLACEMENT_3D('',#21570,#12988,#12989);
#10529=AXIS2_PLACEMENT_3D('',#21574,#12991,#12992);
#10530=AXIS2_PLACEMENT_3D('',#21577,#12994,#12995);
#10531=AXIS2_PLACEMENT_3D('',#21579,#12996,#12997);
#10532=AXIS2_PLACEMENT_3D('',#21581,#12999,#13000);
#10533=AXIS2_PLACEMENT_3D('',#21584,#13001,#13002);
#10534=AXIS2_PLACEMENT_3D('',#21586,#13003,#13004);
#10535=AXIS2_PLACEMENT_3D('',#21587,#13005,#13006);
#10536=AXIS2_PLACEMENT_3D('',#21588,#13007,#13008);
#10537=AXIS2_PLACEMENT_3D('',#21592,#13010,#13011);
#10538=AXIS2_PLACEMENT_3D('',#21596,#13014,#13015);
#10539=AXIS2_PLACEMENT_3D('',#21597,#13016,#13017);
#10540=AXIS2_PLACEMENT_3D('',#21600,#13018,#13019);
#10541=AXIS2_PLACEMENT_3D('',#21602,#13020,#13021);
#10542=AXIS2_PLACEMENT_3D('',#21603,#13022,#13023);
#10543=AXIS2_PLACEMENT_3D('',#21604,#13024,#13025);
#10544=AXIS2_PLACEMENT_3D('',#21608,#13027,#13028);
#10545=AXIS2_PLACEMENT_3D('',#21612,#13031,#13032);
#10546=AXIS2_PLACEMENT_3D('',#21613,#13033,#13034);
#10547=AXIS2_PLACEMENT_3D('',#21615,#13035,#13036);
#10548=AXIS2_PLACEMENT_3D('',#21618,#13038,#13039);
#10549=AXIS2_PLACEMENT_3D('',#21619,#13040,#13041);
#10550=AXIS2_PLACEMENT_3D('',#21620,#13042,#13043);
#10551=AXIS2_PLACEMENT_3D('',#21621,#13044,#13045);
#10552=AXIS2_PLACEMENT_3D('',#21622,#13046,#13047);
#10553=AXIS2_PLACEMENT_3D('',#21623,#13048,#13049);
#10554=AXIS2_PLACEMENT_3D('',#21625,#13050,#13051);
#10555=AXIS2_PLACEMENT_3D('',#21628,#13053,#13054);
#10556=AXIS2_PLACEMENT_3D('',#21629,#13055,#13056);
#10557=AXIS2_PLACEMENT_3D('',#21631,#13057,#13058);
#10558=AXIS2_PLACEMENT_3D('',#21632,#13059,#13060);
#10559=AXIS2_PLACEMENT_3D('',#21634,#13061,#13062);
#10560=AXIS2_PLACEMENT_3D('',#21635,#13063,#13064);
#10561=AXIS2_PLACEMENT_3D('',#21637,#13065,#13066);
#10562=AXIS2_PLACEMENT_3D('',#21639,#13068,#13069);
#10563=AXIS2_PLACEMENT_3D('',#21642,#13071,#13072);
#10564=AXIS2_PLACEMENT_3D('',#21643,#13073,#13074);
#10565=AXIS2_PLACEMENT_3D('',#21644,#13075,#13076);
#10566=AXIS2_PLACEMENT_3D('',#21645,#13077,#13078);
#10567=AXIS2_PLACEMENT_3D('',#21646,#13079,#13080);
#10568=AXIS2_PLACEMENT_3D('',#21649,#13081,#13082);
#10569=AXIS2_PLACEMENT_3D('',#21650,#13083,#13084);
#10570=AXIS2_PLACEMENT_3D('',#21651,#13085,#13086);
#10571=AXIS2_PLACEMENT_3D('',#21655,#13088,#13089);
#10572=AXIS2_PLACEMENT_3D('',#21658,#13091,#13092);
#10573=AXIS2_PLACEMENT_3D('',#21660,#13093,#13094);
#10574=AXIS2_PLACEMENT_3D('',#21662,#13096,#13097);
#10575=AXIS2_PLACEMENT_3D('',#21665,#13098,#13099);
#10576=AXIS2_PLACEMENT_3D('',#21666,#13100,#13101);
#10577=AXIS2_PLACEMENT_3D('',#21667,#13102,#13103);
#10578=AXIS2_PLACEMENT_3D('',#21671,#13105,#13106);
#10579=AXIS2_PLACEMENT_3D('',#21674,#13108,#13109);
#10580=AXIS2_PLACEMENT_3D('',#21676,#13110,#13111);
#10581=AXIS2_PLACEMENT_3D('',#21678,#13113,#13114);
#10582=AXIS2_PLACEMENT_3D('',#21681,#13115,#13116);
#10583=AXIS2_PLACEMENT_3D('',#21683,#13117,#13118);
#10584=AXIS2_PLACEMENT_3D('',#21684,#13119,#13120);
#10585=AXIS2_PLACEMENT_3D('',#21685,#13121,#13122);
#10586=AXIS2_PLACEMENT_3D('',#21689,#13124,#13125);
#10587=AXIS2_PLACEMENT_3D('',#21693,#13128,#13129);
#10588=AXIS2_PLACEMENT_3D('',#21694,#13130,#13131);
#10589=AXIS2_PLACEMENT_3D('',#21697,#13132,#13133);
#10590=AXIS2_PLACEMENT_3D('',#21699,#13134,#13135);
#10591=AXIS2_PLACEMENT_3D('',#21700,#13136,#13137);
#10592=AXIS2_PLACEMENT_3D('',#21701,#13138,#13139);
#10593=AXIS2_PLACEMENT_3D('',#21705,#13141,#13142);
#10594=AXIS2_PLACEMENT_3D('',#21709,#13145,#13146);
#10595=AXIS2_PLACEMENT_3D('',#21710,#13147,#13148);
#10596=AXIS2_PLACEMENT_3D('',#21712,#13149,#13150);
#10597=AXIS2_PLACEMENT_3D('',#21715,#13152,#13153);
#10598=AXIS2_PLACEMENT_3D('',#21716,#13154,#13155);
#10599=AXIS2_PLACEMENT_3D('',#21717,#13156,#13157);
#10600=AXIS2_PLACEMENT_3D('',#21718,#13158,#13159);
#10601=AXIS2_PLACEMENT_3D('',#21719,#13160,#13161);
#10602=AXIS2_PLACEMENT_3D('',#21720,#13162,#13163);
#10603=AXIS2_PLACEMENT_3D('',#21722,#13164,#13165);
#10604=AXIS2_PLACEMENT_3D('',#21725,#13167,#13168);
#10605=AXIS2_PLACEMENT_3D('',#21726,#13169,#13170);
#10606=AXIS2_PLACEMENT_3D('',#21728,#13171,#13172);
#10607=AXIS2_PLACEMENT_3D('',#21729,#13173,#13174);
#10608=AXIS2_PLACEMENT_3D('',#21731,#13175,#13176);
#10609=AXIS2_PLACEMENT_3D('',#21732,#13177,#13178);
#10610=AXIS2_PLACEMENT_3D('',#21734,#13179,#13180);
#10611=AXIS2_PLACEMENT_3D('',#21736,#13182,#13183);
#10612=AXIS2_PLACEMENT_3D('',#21739,#13185,#13186);
#10613=AXIS2_PLACEMENT_3D('',#21740,#13187,#13188);
#10614=AXIS2_PLACEMENT_3D('',#21741,#13189,#13190);
#10615=AXIS2_PLACEMENT_3D('',#21742,#13191,#13192);
#10616=AXIS2_PLACEMENT_3D('',#21743,#13193,#13194);
#10617=AXIS2_PLACEMENT_3D('',#21746,#13195,#13196);
#10618=AXIS2_PLACEMENT_3D('',#21747,#13197,#13198);
#10619=AXIS2_PLACEMENT_3D('',#21748,#13199,#13200);
#10620=AXIS2_PLACEMENT_3D('',#21752,#13202,#13203);
#10621=AXIS2_PLACEMENT_3D('',#21755,#13205,#13206);
#10622=AXIS2_PLACEMENT_3D('',#21757,#13207,#13208);
#10623=AXIS2_PLACEMENT_3D('',#21759,#13210,#13211);
#10624=AXIS2_PLACEMENT_3D('',#21762,#13212,#13213);
#10625=AXIS2_PLACEMENT_3D('',#21763,#13214,#13215);
#10626=AXIS2_PLACEMENT_3D('',#21764,#13216,#13217);
#10627=AXIS2_PLACEMENT_3D('',#21768,#13219,#13220);
#10628=AXIS2_PLACEMENT_3D('',#21771,#13222,#13223);
#10629=AXIS2_PLACEMENT_3D('',#21773,#13224,#13225);
#10630=AXIS2_PLACEMENT_3D('',#21775,#13227,#13228);
#10631=AXIS2_PLACEMENT_3D('',#21778,#13229,#13230);
#10632=AXIS2_PLACEMENT_3D('',#21780,#13231,#13232);
#10633=AXIS2_PLACEMENT_3D('',#21781,#13233,#13234);
#10634=AXIS2_PLACEMENT_3D('',#21782,#13235,#13236);
#10635=AXIS2_PLACEMENT_3D('',#21786,#13238,#13239);
#10636=AXIS2_PLACEMENT_3D('',#21790,#13242,#13243);
#10637=AXIS2_PLACEMENT_3D('',#21791,#13244,#13245);
#10638=AXIS2_PLACEMENT_3D('',#21794,#13246,#13247);
#10639=AXIS2_PLACEMENT_3D('',#21796,#13248,#13249);
#10640=AXIS2_PLACEMENT_3D('',#21797,#13250,#13251);
#10641=AXIS2_PLACEMENT_3D('',#21798,#13252,#13253);
#10642=AXIS2_PLACEMENT_3D('',#21802,#13255,#13256);
#10643=AXIS2_PLACEMENT_3D('',#21806,#13259,#13260);
#10644=AXIS2_PLACEMENT_3D('',#21807,#13261,#13262);
#10645=AXIS2_PLACEMENT_3D('',#21809,#13263,#13264);
#10646=AXIS2_PLACEMENT_3D('',#21812,#13266,#13267);
#10647=AXIS2_PLACEMENT_3D('',#21813,#13268,#13269);
#10648=AXIS2_PLACEMENT_3D('',#21814,#13270,#13271);
#10649=AXIS2_PLACEMENT_3D('',#21815,#13272,#13273);
#10650=AXIS2_PLACEMENT_3D('',#21816,#13274,#13275);
#10651=AXIS2_PLACEMENT_3D('',#21817,#13276,#13277);
#10652=AXIS2_PLACEMENT_3D('',#21819,#13278,#13279);
#10653=AXIS2_PLACEMENT_3D('',#21822,#13281,#13282);
#10654=AXIS2_PLACEMENT_3D('',#21823,#13283,#13284);
#10655=AXIS2_PLACEMENT_3D('',#21825,#13285,#13286);
#10656=AXIS2_PLACEMENT_3D('',#21826,#13287,#13288);
#10657=AXIS2_PLACEMENT_3D('',#21828,#13289,#13290);
#10658=AXIS2_PLACEMENT_3D('',#21829,#13291,#13292);
#10659=AXIS2_PLACEMENT_3D('',#21831,#13293,#13294);
#10660=AXIS2_PLACEMENT_3D('',#21833,#13296,#13297);
#10661=AXIS2_PLACEMENT_3D('',#21836,#13299,#13300);
#10662=AXIS2_PLACEMENT_3D('',#21837,#13301,#13302);
#10663=AXIS2_PLACEMENT_3D('',#21838,#13303,#13304);
#10664=AXIS2_PLACEMENT_3D('',#21839,#13305,#13306);
#10665=AXIS2_PLACEMENT_3D('',#21840,#13307,#13308);
#10666=AXIS2_PLACEMENT_3D('',#21843,#13309,#13310);
#10667=AXIS2_PLACEMENT_3D('',#21844,#13311,#13312);
#10668=AXIS2_PLACEMENT_3D('',#21845,#13313,#13314);
#10669=AXIS2_PLACEMENT_3D('',#21849,#13316,#13317);
#10670=AXIS2_PLACEMENT_3D('',#21852,#13319,#13320);
#10671=AXIS2_PLACEMENT_3D('',#21854,#13321,#13322);
#10672=AXIS2_PLACEMENT_3D('',#21856,#13324,#13325);
#10673=AXIS2_PLACEMENT_3D('',#21859,#13326,#13327);
#10674=AXIS2_PLACEMENT_3D('',#21860,#13328,#13329);
#10675=AXIS2_PLACEMENT_3D('',#21861,#13330,#13331);
#10676=AXIS2_PLACEMENT_3D('',#21865,#13333,#13334);
#10677=AXIS2_PLACEMENT_3D('',#21868,#13336,#13337);
#10678=AXIS2_PLACEMENT_3D('',#21870,#13338,#13339);
#10679=AXIS2_PLACEMENT_3D('',#21872,#13341,#13342);
#10680=AXIS2_PLACEMENT_3D('',#21875,#13343,#13344);
#10681=AXIS2_PLACEMENT_3D('',#21877,#13345,#13346);
#10682=AXIS2_PLACEMENT_3D('',#21878,#13347,#13348);
#10683=AXIS2_PLACEMENT_3D('',#21879,#13349,#13350);
#10684=AXIS2_PLACEMENT_3D('',#21883,#13352,#13353);
#10685=AXIS2_PLACEMENT_3D('',#21887,#13356,#13357);
#10686=AXIS2_PLACEMENT_3D('',#21888,#13358,#13359);
#10687=AXIS2_PLACEMENT_3D('',#21891,#13360,#13361);
#10688=AXIS2_PLACEMENT_3D('',#21893,#13362,#13363);
#10689=AXIS2_PLACEMENT_3D('',#21894,#13364,#13365);
#10690=AXIS2_PLACEMENT_3D('',#21895,#13366,#13367);
#10691=AXIS2_PLACEMENT_3D('',#21899,#13369,#13370);
#10692=AXIS2_PLACEMENT_3D('',#21903,#13373,#13374);
#10693=AXIS2_PLACEMENT_3D('',#21904,#13375,#13376);
#10694=AXIS2_PLACEMENT_3D('',#21906,#13377,#13378);
#10695=AXIS2_PLACEMENT_3D('',#21909,#13380,#13381);
#10696=AXIS2_PLACEMENT_3D('',#21910,#13382,#13383);
#10697=AXIS2_PLACEMENT_3D('',#21911,#13384,#13385);
#10698=AXIS2_PLACEMENT_3D('',#21912,#13386,#13387);
#10699=AXIS2_PLACEMENT_3D('',#21913,#13388,#13389);
#10700=AXIS2_PLACEMENT_3D('',#21914,#13390,#13391);
#10701=AXIS2_PLACEMENT_3D('',#21916,#13392,#13393);
#10702=AXIS2_PLACEMENT_3D('',#21919,#13395,#13396);
#10703=AXIS2_PLACEMENT_3D('',#21920,#13397,#13398);
#10704=AXIS2_PLACEMENT_3D('',#21922,#13399,#13400);
#10705=AXIS2_PLACEMENT_3D('',#21923,#13401,#13402);
#10706=AXIS2_PLACEMENT_3D('',#21925,#13403,#13404);
#10707=AXIS2_PLACEMENT_3D('',#21926,#13405,#13406);
#10708=AXIS2_PLACEMENT_3D('',#21928,#13407,#13408);
#10709=AXIS2_PLACEMENT_3D('',#21930,#13410,#13411);
#10710=AXIS2_PLACEMENT_3D('',#21933,#13413,#13414);
#10711=AXIS2_PLACEMENT_3D('',#21934,#13415,#13416);
#10712=AXIS2_PLACEMENT_3D('',#21935,#13417,#13418);
#10713=AXIS2_PLACEMENT_3D('',#21936,#13419,#13420);
#10714=AXIS2_PLACEMENT_3D('',#21937,#13421,#13422);
#10715=AXIS2_PLACEMENT_3D('',#21939,#13423,#13424);
#10716=AXIS2_PLACEMENT_3D('',#21942,#13426,#13427);
#10717=AXIS2_PLACEMENT_3D('',#21943,#13428,#13429);
#10718=AXIS2_PLACEMENT_3D('',#21945,#13430,#13431);
#10719=AXIS2_PLACEMENT_3D('',#21948,#13433,#13434);
#10720=AXIS2_PLACEMENT_3D('',#21949,#13435,#13436);
#10721=AXIS2_PLACEMENT_3D('',#21951,#13437,#13438);
#10722=AXIS2_PLACEMENT_3D('',#21954,#13440,#13441);
#10723=AXIS2_PLACEMENT_3D('',#21955,#13442,#13443);
#10724=AXIS2_PLACEMENT_3D('',#21957,#13444,#13445);
#10725=AXIS2_PLACEMENT_3D('',#21960,#13447,#13448);
#10726=AXIS2_PLACEMENT_3D('',#21961,#13449,#13450);
#10727=AXIS2_PLACEMENT_3D('',#21963,#13451,#13452);
#10728=AXIS2_PLACEMENT_3D('',#21965,#13453,#13454);
#10729=AXIS2_PLACEMENT_3D('',#21966,#13455,#13456);
#10730=AXIS2_PLACEMENT_3D('',#21968,#13457,#13458);
#10731=AXIS2_PLACEMENT_3D('',#21970,#13460,#13461);
#10732=AXIS2_PLACEMENT_3D('',#21973,#13463,#13464);
#10733=AXIS2_PLACEMENT_3D('',#21974,#13465,#13466);
#10734=AXIS2_PLACEMENT_3D('',#21975,#13467,#13468);
#10735=AXIS2_PLACEMENT_3D('',#21976,#13469,#13470);
#10736=AXIS2_PLACEMENT_3D('',#21977,#13471,#13472);
#10737=AXIS2_PLACEMENT_3D('',#21978,#13473,#13474);
#10738=AXIS2_PLACEMENT_3D('',#21981,#13475,#13476);
#10739=AXIS2_PLACEMENT_3D('',#21987,#13480,#13481);
#10740=AXIS2_PLACEMENT_3D('',#21993,#13485,#13486);
#10741=AXIS2_PLACEMENT_3D('',#21995,#13487,#13488);
#10742=AXIS2_PLACEMENT_3D('',#21999,#13491,#13492);
#10743=AXIS2_PLACEMENT_3D('',#22002,#13495,#13496);
#10744=AXIS2_PLACEMENT_3D('',#22003,#13497,#13498);
#10745=AXIS2_PLACEMENT_3D('',#22005,#13499,#13500);
#10746=AXIS2_PLACEMENT_3D('',#22007,#13501,#13502);
#10747=AXIS2_PLACEMENT_3D('',#22008,#13503,#13504);
#10748=AXIS2_PLACEMENT_3D('',#22010,#13505,#13506);
#10749=AXIS2_PLACEMENT_3D('',#22012,#13508,#13509);
#10750=AXIS2_PLACEMENT_3D('',#22014,#13510,#13511);
#10751=AXIS2_PLACEMENT_3D('',#22015,#13512,#13513);
#10752=AXIS2_PLACEMENT_3D('',#22017,#13514,#13515);
#10753=AXIS2_PLACEMENT_3D('',#22019,#13517,#13518);
#10754=AXIS2_PLACEMENT_3D('',#22021,#13519,#13520);
#10755=AXIS2_PLACEMENT_3D('',#22022,#13521,#13522);
#10756=AXIS2_PLACEMENT_3D('',#22024,#13523,#13524);
#10757=AXIS2_PLACEMENT_3D('',#22026,#13526,#13527);
#10758=AXIS2_PLACEMENT_3D('',#22028,#13528,#13529);
#10759=AXIS2_PLACEMENT_3D('',#22029,#13530,#13531);
#10760=AXIS2_PLACEMENT_3D('',#22031,#13532,#13533);
#10761=AXIS2_PLACEMENT_3D('',#22033,#13535,#13536);
#10762=AXIS2_PLACEMENT_3D('',#22035,#13537,#13538);
#10763=AXIS2_PLACEMENT_3D('',#22036,#13539,#13540);
#10764=AXIS2_PLACEMENT_3D('',#22038,#13541,#13542);
#10765=AXIS2_PLACEMENT_3D('',#22040,#13544,#13545);
#10766=AXIS2_PLACEMENT_3D('',#22042,#13546,#13547);
#10767=AXIS2_PLACEMENT_3D('',#22043,#13548,#13549);
#10768=AXIS2_PLACEMENT_3D('',#22045,#13551,#13552);
#10769=AXIS2_PLACEMENT_3D('',#22046,#13553,#13554);
#10770=AXIS2_PLACEMENT_3D('',#22049,#13555,#13556);
#10771=AXIS2_PLACEMENT_3D('',#22053,#13558,#13559);
#10772=AXIS2_PLACEMENT_3D('',#22055,#13561,#13562);
#10773=AXIS2_PLACEMENT_3D('',#22061,#13566,#13567);
#10774=AXIS2_PLACEMENT_3D('',#22063,#13568,#13569);
#10775=AXIS2_PLACEMENT_3D('',#22065,#13570,#13571);
#10776=AXIS2_PLACEMENT_3D('',#22067,#13573,#13574);
#10777=AXIS2_PLACEMENT_3D('',#22070,#13577,#13578);
#10778=AXIS2_PLACEMENT_3D('',#22072,#13579,#13580);
#10779=AXIS2_PLACEMENT_3D('',#22074,#13581,#13582);
#10780=AXIS2_PLACEMENT_3D('',#22075,#13583,#13584);
#10781=AXIS2_PLACEMENT_3D('',#22077,#13585,#13586);
#10782=AXIS2_PLACEMENT_3D('',#22079,#13588,#13589);
#10783=AXIS2_PLACEMENT_3D('',#22081,#13590,#13591);
#10784=AXIS2_PLACEMENT_3D('',#22082,#13592,#13593);
#10785=AXIS2_PLACEMENT_3D('',#22084,#13595,#13596);
#10786=AXIS2_PLACEMENT_3D('',#22085,#13597,#13598);
#10787=AXIS2_PLACEMENT_3D('',#22086,#13599,#13600);
#10788=AXIS2_PLACEMENT_3D('',#22087,#13601,#13602);
#10789=AXIS2_PLACEMENT_3D('',#22089,#13603,#13604);
#10790=AXIS2_PLACEMENT_3D('',#22090,#13605,#13606);
#10791=AXIS2_PLACEMENT_3D('',#22092,#13607,#13608);
#10792=AXIS2_PLACEMENT_3D('',#22094,#13610,#13611);
#10793=AXIS2_PLACEMENT_3D('',#22096,#13612,#13613);
#10794=AXIS2_PLACEMENT_3D('',#22098,#13615,#13616);
#10795=AXIS2_PLACEMENT_3D('',#22100,#13617,#13618);
#10796=AXIS2_PLACEMENT_3D('',#22102,#13620,#13621);
#10797=AXIS2_PLACEMENT_3D('',#22104,#13622,#13623);
#10798=AXIS2_PLACEMENT_3D('',#22105,#13624,#13625);
#10799=AXIS2_PLACEMENT_3D('',#22107,#13626,#13627);
#10800=AXIS2_PLACEMENT_3D('',#22109,#13629,#13630);
#10801=AXIS2_PLACEMENT_3D('',#22111,#13631,#13632);
#10802=AXIS2_PLACEMENT_3D('',#22113,#13634,#13635);
#10803=AXIS2_PLACEMENT_3D('',#22115,#13636,#13637);
#10804=AXIS2_PLACEMENT_3D('',#22117,#13639,#13640);
#10805=AXIS2_PLACEMENT_3D('',#22118,#13641,#13642);
#10806=AXIS2_PLACEMENT_3D('',#22127,#13647,#13648);
#10807=AXIS2_PLACEMENT_3D('',#22133,#13652,#13653);
#10808=AXIS2_PLACEMENT_3D('',#22139,#13657,#13658);
#10809=AXIS2_PLACEMENT_3D('',#22145,#13662,#13663);
#10810=AXIS2_PLACEMENT_3D('',#22151,#13667,#13668);
#10811=AXIS2_PLACEMENT_3D('',#22154,#13671,#13672);
#10812=AXIS2_PLACEMENT_3D('',#22155,#13673,#13674);
#10813=AXIS2_PLACEMENT_3D('',#22156,#13675,#13676);
#10814=AXIS2_PLACEMENT_3D('',#22157,#13677,#13678);
#10815=AXIS2_PLACEMENT_3D('',#22158,#13679,#13680);
#10816=AXIS2_PLACEMENT_3D('',#22159,#13681,#13682);
#10817=AXIS2_PLACEMENT_3D('',#22160,#13683,#13684);
#10818=AXIS2_PLACEMENT_3D('',#22161,#13685,#13686);
#10819=AXIS2_PLACEMENT_3D('',#22162,#13687,#13688);
#10820=AXIS2_PLACEMENT_3D('',#22163,#13689,#13690);
#10821=AXIS2_PLACEMENT_3D('',#22164,#13691,#13692);
#10822=AXIS2_PLACEMENT_3D('',#22165,#13693,#13694);
#10823=AXIS2_PLACEMENT_3D('',#22166,#13695,#13696);
#10824=AXIS2_PLACEMENT_3D('',#22167,#13697,#13698);
#10825=AXIS2_PLACEMENT_3D('',#22168,#13699,#13700);
#10826=AXIS2_PLACEMENT_3D('',#22169,#13701,#13702);
#10827=AXIS2_PLACEMENT_3D('',#22170,#13703,#13704);
#10828=AXIS2_PLACEMENT_3D('',#22171,#13705,#13706);
#10829=AXIS2_PLACEMENT_3D('',#22172,#13707,#13708);
#10830=AXIS2_PLACEMENT_3D('',#22173,#13709,#13710);
#10831=AXIS2_PLACEMENT_3D('',#22174,#13711,#13712);
#10832=AXIS2_PLACEMENT_3D('',#22175,#13713,#13714);
#10833=AXIS2_PLACEMENT_3D('',#22176,#13715,#13716);
#10834=AXIS2_PLACEMENT_3D('',#22177,#13717,#13718);
#10835=AXIS2_PLACEMENT_3D('',#22178,#13719,#13720);
#10836=AXIS2_PLACEMENT_3D('',#22179,#13721,#13722);
#10837=AXIS2_PLACEMENT_3D('',#22180,#13723,#13724);
#10838=AXIS2_PLACEMENT_3D('',#22181,#13725,#13726);
#10839=AXIS2_PLACEMENT_3D('',#22182,#13727,#13728);
#10840=AXIS2_PLACEMENT_3D('',#22183,#13729,#13730);
#10841=AXIS2_PLACEMENT_3D('',#22184,#13731,#13732);
#10842=AXIS2_PLACEMENT_3D('',#22185,#13733,#13734);
#10843=AXIS2_PLACEMENT_3D('',#22186,#13735,#13736);
#10844=AXIS2_PLACEMENT_3D('',#22187,#13737,#13738);
#10845=AXIS2_PLACEMENT_3D('',#22188,#13739,#13740);
#10846=AXIS2_PLACEMENT_3D('',#22189,#13741,#13742);
#10847=AXIS2_PLACEMENT_3D('',#22190,#13743,#13744);
#10848=AXIS2_PLACEMENT_3D('',#22191,#13745,#13746);
#10849=AXIS2_PLACEMENT_3D('',#22192,#13747,#13748);
#10850=AXIS2_PLACEMENT_3D('',#22193,#13749,#13750);
#10851=AXIS2_PLACEMENT_3D('',#22194,#13751,#13752);
#10852=AXIS2_PLACEMENT_3D('',#22195,#13753,#13754);
#10853=AXIS2_PLACEMENT_3D('',#22196,#13755,#13756);
#10854=AXIS2_PLACEMENT_3D('',#22197,#13757,#13758);
#10855=AXIS2_PLACEMENT_3D('',#22198,#13759,#13760);
#10856=AXIS2_PLACEMENT_3D('',#22199,#13761,#13762);
#10857=AXIS2_PLACEMENT_3D('',#22200,#13763,#13764);
#10858=AXIS2_PLACEMENT_3D('',#22201,#13765,#13766);
#10859=AXIS2_PLACEMENT_3D('',#22202,#13767,#13768);
#10860=AXIS2_PLACEMENT_3D('',#22203,#13769,#13770);
#10861=AXIS2_PLACEMENT_3D('',#22204,#13771,#13772);
#10862=AXIS2_PLACEMENT_3D('',#22205,#13773,#13774);
#10863=AXIS2_PLACEMENT_3D('',#22206,#13775,#13776);
#10864=AXIS2_PLACEMENT_3D('',#22207,#13777,#13778);
#10865=AXIS2_PLACEMENT_3D('',#22208,#13779,#13780);
#10866=AXIS2_PLACEMENT_3D('',#22209,#13781,#13782);
#10867=AXIS2_PLACEMENT_3D('',#22210,#13783,#13784);
#10868=AXIS2_PLACEMENT_3D('',#22211,#13785,#13786);
#10869=AXIS2_PLACEMENT_3D('',#22212,#13787,#13788);
#10870=AXIS2_PLACEMENT_3D('',#22213,#13789,#13790);
#10871=AXIS2_PLACEMENT_3D('',#22214,#13791,#13792);
#10872=AXIS2_PLACEMENT_3D('',#22215,#13793,#13794);
#10873=AXIS2_PLACEMENT_3D('',#22216,#13795,#13796);
#10874=AXIS2_PLACEMENT_3D('',#22217,#13797,#13798);
#10875=AXIS2_PLACEMENT_3D('',#22218,#13799,#13800);
#10876=AXIS2_PLACEMENT_3D('',#22219,#13801,#13802);
#10877=AXIS2_PLACEMENT_3D('',#22220,#13803,#13804);
#10878=AXIS2_PLACEMENT_3D('',#22221,#13805,#13806);
#10879=AXIS2_PLACEMENT_3D('',#22222,#13807,#13808);
#10880=AXIS2_PLACEMENT_3D('',#22223,#13809,#13810);
#10881=AXIS2_PLACEMENT_3D('',#22224,#13811,#13812);
#10882=AXIS2_PLACEMENT_3D('',#22225,#13813,#13814);
#10883=AXIS2_PLACEMENT_3D('',#22226,#13815,#13816);
#10884=AXIS2_PLACEMENT_3D('',#22227,#13817,#13818);
#10885=AXIS2_PLACEMENT_3D('',#22228,#13819,#13820);
#10886=AXIS2_PLACEMENT_3D('',#22229,#13821,#13822);
#10887=AXIS2_PLACEMENT_3D('',#22230,#13823,#13824);
#10888=AXIS2_PLACEMENT_3D('',#22231,#13825,#13826);
#10889=AXIS2_PLACEMENT_3D('',#22232,#13827,#13828);
#10890=AXIS2_PLACEMENT_3D('',#22233,#13829,#13830);
#10891=AXIS2_PLACEMENT_3D('',#22234,#13831,#13832);
#10892=AXIS2_PLACEMENT_3D('',#22235,#13833,#13834);
#10893=AXIS2_PLACEMENT_3D('',#22236,#13835,#13836);
#10894=AXIS2_PLACEMENT_3D('',#22237,#13837,#13838);
#10895=AXIS2_PLACEMENT_3D('',#22238,#13839,#13840);
#10896=AXIS2_PLACEMENT_3D('',#22239,#13841,#13842);
#10897=AXIS2_PLACEMENT_3D('',#22240,#13843,#13844);
#10898=AXIS2_PLACEMENT_3D('',#22241,#13845,#13846);
#10899=AXIS2_PLACEMENT_3D('',#22242,#13847,#13848);
#10900=AXIS2_PLACEMENT_3D('',#22243,#13849,#13850);
#10901=AXIS2_PLACEMENT_3D('',#22244,#13851,#13852);
#10902=AXIS2_PLACEMENT_3D('',#22245,#13853,#13854);
#10903=AXIS2_PLACEMENT_3D('',#22246,#13855,#13856);
#10904=AXIS2_PLACEMENT_3D('',#22247,#13857,#13858);
#10905=AXIS2_PLACEMENT_3D('',#22248,#13859,#13860);
#10906=AXIS2_PLACEMENT_3D('',#22249,#13861,#13862);
#10907=AXIS2_PLACEMENT_3D('',#22250,#13863,#13864);
#10908=AXIS2_PLACEMENT_3D('',#22251,#13865,#13866);
#10909=AXIS2_PLACEMENT_3D('',#22252,#13867,#13868);
#10910=AXIS2_PLACEMENT_3D('',#22253,#13869,#13870);
#10911=AXIS2_PLACEMENT_3D('',#22254,#13871,#13872);
#10912=AXIS2_PLACEMENT_3D('',#22255,#13873,#13874);
#10913=AXIS2_PLACEMENT_3D('',#22256,#13875,#13876);
#10914=AXIS2_PLACEMENT_3D('',#22257,#13877,#13878);
#10915=AXIS2_PLACEMENT_3D('',#22258,#13879,#13880);
#10916=AXIS2_PLACEMENT_3D('',#22259,#13881,#13882);
#10917=AXIS2_PLACEMENT_3D('',#22260,#13883,#13884);
#10918=AXIS2_PLACEMENT_3D('',#22261,#13885,#13886);
#10919=AXIS2_PLACEMENT_3D('',#22262,#13887,#13888);
#10920=AXIS2_PLACEMENT_3D('',#22263,#13889,#13890);
#10921=AXIS2_PLACEMENT_3D('',#22264,#13891,#13892);
#10922=AXIS2_PLACEMENT_3D('',#22265,#13893,#13894);
#10923=AXIS2_PLACEMENT_3D('',#22266,#13895,#13896);
#10924=AXIS2_PLACEMENT_3D('',#22267,#13897,#13898);
#10925=AXIS2_PLACEMENT_3D('',#22268,#13899,#13900);
#10926=AXIS2_PLACEMENT_3D('',#22269,#13901,#13902);
#10927=AXIS2_PLACEMENT_3D('',#22270,#13903,#13904);
#10928=AXIS2_PLACEMENT_3D('',#22271,#13905,#13906);
#10929=AXIS2_PLACEMENT_3D('',#22272,#13907,#13908);
#10930=AXIS2_PLACEMENT_3D('',#22273,#13909,#13910);
#10931=AXIS2_PLACEMENT_3D('',#22274,#13911,#13912);
#10932=AXIS2_PLACEMENT_3D('',#22275,#13913,#13914);
#10933=AXIS2_PLACEMENT_3D('',#22276,#13915,#13916);
#10934=AXIS2_PLACEMENT_3D('',#22277,#13917,#13918);
#10935=AXIS2_PLACEMENT_3D('',#22278,#13919,#13920);
#10936=AXIS2_PLACEMENT_3D('',#22279,#13921,#13922);
#10937=AXIS2_PLACEMENT_3D('',#22280,#13923,#13924);
#10938=AXIS2_PLACEMENT_3D('',#22281,#13925,#13926);
#10939=AXIS2_PLACEMENT_3D('',#22282,#13927,#13928);
#10940=AXIS2_PLACEMENT_3D('',#22283,#13929,#13930);
#10941=AXIS2_PLACEMENT_3D('',#22284,#13931,#13932);
#10942=AXIS2_PLACEMENT_3D('',#22285,#13933,#13934);
#10943=AXIS2_PLACEMENT_3D('',#22286,#13935,#13936);
#10944=AXIS2_PLACEMENT_3D('',#22287,#13937,#13938);
#10945=AXIS2_PLACEMENT_3D('',#22288,#13939,#13940);
#10946=AXIS2_PLACEMENT_3D('',#22289,#13941,#13942);
#10947=AXIS2_PLACEMENT_3D('',#22290,#13943,#13944);
#10948=AXIS2_PLACEMENT_3D('',#22291,#13945,#13946);
#10949=AXIS2_PLACEMENT_3D('',#22292,#13947,#13948);
#10950=DIRECTION('axis',(0.,0.,1.));
#10951=DIRECTION('refdir',(1.,0.,0.));
#10952=DIRECTION('axis',(0.,0.,1.));
#10953=DIRECTION('refdir',(1.,0.,0.));
#10954=DIRECTION('axis',(0.,0.,1.));
#10955=DIRECTION('refdir',(1.,0.,0.));
#10956=DIRECTION('center_axis',(0.,0.,1.));
#10957=DIRECTION('ref_axis',(1.,0.,0.));
#10958=DIRECTION('center_axis',(0.,0.,1.));
#10959=DIRECTION('ref_axis',(1.,0.,0.));
#10960=DIRECTION('',(0.,0.,1.));
#10961=DIRECTION('center_axis',(0.,0.,-1.));
#10962=DIRECTION('ref_axis',(1.,0.,0.));
#10963=DIRECTION('center_axis',(0.,0.,1.));
#10964=DIRECTION('ref_axis',(1.,0.,0.));
#10965=DIRECTION('center_axis',(0.,0.,1.));
#10966=DIRECTION('ref_axis',(1.,0.,0.));
#10967=DIRECTION('',(0.,0.,1.));
#10968=DIRECTION('center_axis',(0.,0.,-1.));
#10969=DIRECTION('ref_axis',(1.,0.,0.));
#10970=DIRECTION('center_axis',(0.,0.,1.));
#10971=DIRECTION('ref_axis',(1.,0.,0.));
#10972=DIRECTION('center_axis',(0.,0.,1.));
#10973=DIRECTION('ref_axis',(1.,0.,0.));
#10974=DIRECTION('',(0.,0.,1.));
#10975=DIRECTION('center_axis',(0.,0.,-1.));
#10976=DIRECTION('ref_axis',(1.,0.,0.));
#10977=DIRECTION('center_axis',(0.,0.,1.));
#10978=DIRECTION('ref_axis',(1.,0.,0.));
#10979=DIRECTION('center_axis',(0.,0.,1.));
#10980=DIRECTION('ref_axis',(1.,0.,0.));
#10981=DIRECTION('',(0.,0.,1.));
#10982=DIRECTION('center_axis',(0.,0.,-1.));
#10983=DIRECTION('ref_axis',(1.,0.,0.));
#10984=DIRECTION('center_axis',(0.,0.,1.));
#10985=DIRECTION('ref_axis',(1.,0.,0.));
#10986=DIRECTION('center_axis',(0.,0.,1.));
#10987=DIRECTION('ref_axis',(1.,0.,0.));
#10988=DIRECTION('',(0.,0.,1.));
#10989=DIRECTION('center_axis',(0.,0.,-1.));
#10990=DIRECTION('ref_axis',(1.,0.,0.));
#10991=DIRECTION('center_axis',(0.,0.,1.));
#10992=DIRECTION('ref_axis',(1.,0.,0.));
#10993=DIRECTION('center_axis',(0.,0.,1.));
#10994=DIRECTION('ref_axis',(1.,0.,0.));
#10995=DIRECTION('',(0.,0.,1.));
#10996=DIRECTION('center_axis',(0.,0.,-1.));
#10997=DIRECTION('ref_axis',(1.,0.,0.));
#10998=DIRECTION('center_axis',(0.,0.,1.));
#10999=DIRECTION('ref_axis',(1.,0.,0.));
#11000=DIRECTION('center_axis',(0.,0.,1.));
#11001=DIRECTION('ref_axis',(1.,0.,0.));
#11002=DIRECTION('',(0.,0.,1.));
#11003=DIRECTION('center_axis',(0.,0.,-1.));
#11004=DIRECTION('ref_axis',(1.,0.,0.));
#11005=DIRECTION('center_axis',(0.,0.,1.));
#11006=DIRECTION('ref_axis',(1.,0.,0.));
#11007=DIRECTION('center_axis',(0.,0.,1.));
#11008=DIRECTION('ref_axis',(1.,0.,0.));
#11009=DIRECTION('',(0.,0.,1.));
#11010=DIRECTION('center_axis',(0.,0.,-1.));
#11011=DIRECTION('ref_axis',(1.,0.,0.));
#11012=DIRECTION('center_axis',(0.,0.,1.));
#11013=DIRECTION('ref_axis',(1.,0.,0.));
#11014=DIRECTION('center_axis',(0.,0.,1.));
#11015=DIRECTION('ref_axis',(1.,0.,0.));
#11016=DIRECTION('',(0.,0.,1.));
#11017=DIRECTION('center_axis',(0.,0.,-1.));
#11018=DIRECTION('ref_axis',(1.,0.,0.));
#11019=DIRECTION('center_axis',(0.,0.,1.));
#11020=DIRECTION('ref_axis',(1.,0.,0.));
#11021=DIRECTION('center_axis',(0.,0.,1.));
#11022=DIRECTION('ref_axis',(1.,0.,0.));
#11023=DIRECTION('',(0.,0.,1.));
#11024=DIRECTION('center_axis',(0.,0.,-1.));
#11025=DIRECTION('ref_axis',(1.,0.,0.));
#11026=DIRECTION('center_axis',(0.,0.,1.));
#11027=DIRECTION('ref_axis',(1.,0.,0.));
#11028=DIRECTION('center_axis',(0.,0.,1.));
#11029=DIRECTION('ref_axis',(1.,0.,0.));
#11030=DIRECTION('',(0.,0.,1.));
#11031=DIRECTION('center_axis',(0.,0.,-1.));
#11032=DIRECTION('ref_axis',(1.,0.,0.));
#11033=DIRECTION('center_axis',(0.,0.,1.));
#11034=DIRECTION('ref_axis',(1.,0.,0.));
#11035=DIRECTION('center_axis',(0.,0.,1.));
#11036=DIRECTION('ref_axis',(1.,0.,0.));
#11037=DIRECTION('',(0.,0.,1.));
#11038=DIRECTION('center_axis',(0.,0.,-1.));
#11039=DIRECTION('ref_axis',(1.,0.,0.));
#11040=DIRECTION('center_axis',(0.,0.,1.));
#11041=DIRECTION('ref_axis',(1.,0.,0.));
#11042=DIRECTION('center_axis',(0.,0.,1.));
#11043=DIRECTION('ref_axis',(1.,0.,0.));
#11044=DIRECTION('',(0.,0.,1.));
#11045=DIRECTION('center_axis',(0.,0.,-1.));
#11046=DIRECTION('ref_axis',(1.,0.,0.));
#11047=DIRECTION('center_axis',(0.,0.,1.));
#11048=DIRECTION('ref_axis',(1.,0.,0.));
#11049=DIRECTION('center_axis',(0.,0.,1.));
#11050=DIRECTION('ref_axis',(1.,0.,0.));
#11051=DIRECTION('',(0.,0.,1.));
#11052=DIRECTION('center_axis',(0.,0.,-1.));
#11053=DIRECTION('ref_axis',(1.,0.,0.));
#11054=DIRECTION('center_axis',(0.,0.,1.));
#11055=DIRECTION('ref_axis',(1.,0.,0.));
#11056=DIRECTION('center_axis',(0.,0.,1.));
#11057=DIRECTION('ref_axis',(1.,0.,0.));
#11058=DIRECTION('',(0.,0.,1.));
#11059=DIRECTION('center_axis',(0.,0.,-1.));
#11060=DIRECTION('ref_axis',(1.,0.,0.));
#11061=DIRECTION('center_axis',(0.,0.,1.));
#11062=DIRECTION('ref_axis',(1.,0.,0.));
#11063=DIRECTION('center_axis',(0.,0.,1.));
#11064=DIRECTION('ref_axis',(1.,0.,0.));
#11065=DIRECTION('',(0.,0.,1.));
#11066=DIRECTION('center_axis',(0.,0.,-1.));
#11067=DIRECTION('ref_axis',(1.,0.,0.));
#11068=DIRECTION('center_axis',(0.,0.,1.));
#11069=DIRECTION('ref_axis',(1.,0.,0.));
#11070=DIRECTION('center_axis',(0.,0.,1.));
#11071=DIRECTION('ref_axis',(1.,0.,0.));
#11072=DIRECTION('',(0.,0.,1.));
#11073=DIRECTION('center_axis',(0.,0.,-1.));
#11074=DIRECTION('ref_axis',(1.,0.,0.));
#11075=DIRECTION('center_axis',(0.,0.,1.));
#11076=DIRECTION('ref_axis',(1.,0.,0.));
#11077=DIRECTION('center_axis',(0.,0.,1.));
#11078=DIRECTION('ref_axis',(1.,0.,0.));
#11079=DIRECTION('',(0.,0.,1.));
#11080=DIRECTION('center_axis',(0.,0.,-1.));
#11081=DIRECTION('ref_axis',(1.,0.,0.));
#11082=DIRECTION('center_axis',(0.,0.,1.));
#11083=DIRECTION('ref_axis',(1.,0.,0.));
#11084=DIRECTION('center_axis',(0.,0.,1.));
#11085=DIRECTION('ref_axis',(1.,0.,0.));
#11086=DIRECTION('',(0.,0.,1.));
#11087=DIRECTION('center_axis',(0.,0.,-1.));
#11088=DIRECTION('ref_axis',(1.,0.,0.));
#11089=DIRECTION('center_axis',(0.,0.,1.));
#11090=DIRECTION('ref_axis',(1.,0.,0.));
#11091=DIRECTION('center_axis',(0.,0.,1.));
#11092=DIRECTION('ref_axis',(1.,0.,0.));
#11093=DIRECTION('',(0.,0.,1.));
#11094=DIRECTION('center_axis',(0.,0.,-1.));
#11095=DIRECTION('ref_axis',(1.,0.,0.));
#11096=DIRECTION('center_axis',(0.,0.,1.));
#11097=DIRECTION('ref_axis',(1.,0.,0.));
#11098=DIRECTION('center_axis',(0.,0.,1.));
#11099=DIRECTION('ref_axis',(1.,0.,0.));
#11100=DIRECTION('',(0.,0.,1.));
#11101=DIRECTION('center_axis',(0.,0.,-1.));
#11102=DIRECTION('ref_axis',(1.,0.,0.));
#11103=DIRECTION('center_axis',(0.,0.,1.));
#11104=DIRECTION('ref_axis',(1.,0.,0.));
#11105=DIRECTION('center_axis',(0.,0.,1.));
#11106=DIRECTION('ref_axis',(1.,0.,0.));
#11107=DIRECTION('',(0.,0.,1.));
#11108=DIRECTION('center_axis',(0.,0.,-1.));
#11109=DIRECTION('ref_axis',(1.,0.,0.));
#11110=DIRECTION('center_axis',(0.,1.,0.));
#11111=DIRECTION('ref_axis',(-1.,0.,0.));
#11112=DIRECTION('',(-1.,0.,0.));
#11113=DIRECTION('',(0.,0.,1.));
#11114=DIRECTION('',(-1.,0.,0.));
#11115=DIRECTION('',(0.,0.,1.));
#11116=DIRECTION('center_axis',(1.,0.,0.));
#11117=DIRECTION('ref_axis',(0.,1.,0.));
#11118=DIRECTION('',(0.,1.,0.));
#11119=DIRECTION('',(0.,1.,0.));
#11120=DIRECTION('',(0.,0.,1.));
#11121=DIRECTION('center_axis',(0.,-1.,0.));
#11122=DIRECTION('ref_axis',(1.,0.,0.));
#11123=DIRECTION('',(1.,0.,0.));
#11124=DIRECTION('',(1.,0.,0.));
#11125=DIRECTION('',(0.,0.,1.));
#11126=DIRECTION('center_axis',(-1.,0.,0.));
#11127=DIRECTION('ref_axis',(0.,-1.,0.));
#11128=DIRECTION('',(0.,-1.,0.));
#11129=DIRECTION('',(0.,-1.,0.));
#11130=DIRECTION('center_axis',(0.,0.,1.));
#11131=DIRECTION('ref_axis',(1.,0.,0.));
#11132=DIRECTION('center_axis',(0.,0.,1.));
#11133=DIRECTION('ref_axis',(1.,0.,0.));
#11134=DIRECTION('axis',(0.,0.,1.));
#11135=DIRECTION('refdir',(1.,0.,0.));
#11136=DIRECTION('center_axis',(0.,1.,0.));
#11137=DIRECTION('ref_axis',(-1.,0.,0.));
#11138=DIRECTION('',(-1.,0.,0.));
#11139=DIRECTION('',(0.,0.,1.));
#11140=DIRECTION('',(-1.,0.,0.));
#11141=DIRECTION('',(0.,0.,1.));
#11142=DIRECTION('center_axis',(1.,0.,0.));
#11143=DIRECTION('ref_axis',(0.,1.,0.));
#11144=DIRECTION('',(0.,1.,0.));
#11145=DIRECTION('',(0.,1.,0.));
#11146=DIRECTION('',(0.,0.,1.));
#11147=DIRECTION('center_axis',(0.,-1.,0.));
#11148=DIRECTION('ref_axis',(1.,0.,0.));
#11149=DIRECTION('',(1.,0.,0.));
#11150=DIRECTION('',(1.,0.,0.));
#11151=DIRECTION('',(0.,0.,1.));
#11152=DIRECTION('center_axis',(-1.,0.,0.));
#11153=DIRECTION('ref_axis',(0.,-1.,0.));
#11154=DIRECTION('',(0.,-1.,0.));
#11155=DIRECTION('',(0.,-1.,0.));
#11156=DIRECTION('center_axis',(0.,0.,1.));
#11157=DIRECTION('ref_axis',(1.,0.,0.));
#11158=DIRECTION('center_axis',(0.,0.,1.));
#11159=DIRECTION('ref_axis',(1.,0.,0.));
#11160=DIRECTION('axis',(0.,0.,1.));
#11161=DIRECTION('refdir',(1.,0.,0.));
#11162=DIRECTION('center_axis',(0.,1.,0.));
#11163=DIRECTION('ref_axis',(-1.,0.,0.));
#11164=DIRECTION('',(-1.,0.,0.));
#11165=DIRECTION('',(0.,0.,1.));
#11166=DIRECTION('',(-1.,0.,0.));
#11167=DIRECTION('',(0.,0.,1.));
#11168=DIRECTION('center_axis',(1.,0.,0.));
#11169=DIRECTION('ref_axis',(0.,1.,0.));
#11170=DIRECTION('',(0.,1.,0.));
#11171=DIRECTION('',(0.,1.,0.));
#11172=DIRECTION('',(0.,0.,1.));
#11173=DIRECTION('center_axis',(0.,-1.,0.));
#11174=DIRECTION('ref_axis',(1.,0.,0.));
#11175=DIRECTION('',(1.,0.,0.));
#11176=DIRECTION('',(1.,0.,0.));
#11177=DIRECTION('',(0.,0.,1.));
#11178=DIRECTION('center_axis',(-1.,0.,0.));
#11179=DIRECTION('ref_axis',(0.,-1.,0.));
#11180=DIRECTION('',(0.,-1.,0.));
#11181=DIRECTION('',(0.,-1.,0.));
#11182=DIRECTION('center_axis',(0.,0.,1.));
#11183=DIRECTION('ref_axis',(1.,0.,0.));
#11184=DIRECTION('center_axis',(0.,0.,1.));
#11185=DIRECTION('ref_axis',(1.,0.,0.));
#11186=DIRECTION('axis',(0.,0.,1.));
#11187=DIRECTION('refdir',(1.,0.,0.));
#11188=DIRECTION('center_axis',(0.,0.,1.));
#11189=DIRECTION('ref_axis',(1.,0.,0.));
#11190=DIRECTION('center_axis',(0.,0.,1.));
#11191=DIRECTION('ref_axis',(1.,0.,0.));
#11192=DIRECTION('',(0.,0.,1.));
#11193=DIRECTION('center_axis',(0.,0.,-1.));
#11194=DIRECTION('ref_axis',(1.,0.,0.));
#11195=DIRECTION('center_axis',(0.,0.,1.));
#11196=DIRECTION('ref_axis',(1.,0.,0.));
#11197=DIRECTION('center_axis',(0.,0.,1.));
#11198=DIRECTION('ref_axis',(1.,0.,0.));
#11199=DIRECTION('',(0.,0.,1.));
#11200=DIRECTION('center_axis',(0.,0.,-1.));
#11201=DIRECTION('ref_axis',(1.,0.,0.));
#11202=DIRECTION('center_axis',(0.,0.,1.));
#11203=DIRECTION('ref_axis',(1.,0.,0.));
#11204=DIRECTION('center_axis',(0.,0.,1.));
#11205=DIRECTION('ref_axis',(1.,0.,0.));
#11206=DIRECTION('',(0.,0.,1.));
#11207=DIRECTION('center_axis',(0.,0.,-1.));
#11208=DIRECTION('ref_axis',(1.,0.,0.));
#11209=DIRECTION('center_axis',(0.,0.,1.));
#11210=DIRECTION('ref_axis',(1.,0.,0.));
#11211=DIRECTION('center_axis',(0.,0.,1.));
#11212=DIRECTION('ref_axis',(1.,0.,0.));
#11213=DIRECTION('',(0.,0.,1.));
#11214=DIRECTION('center_axis',(0.,0.,-1.));
#11215=DIRECTION('ref_axis',(1.,0.,0.));
#11216=DIRECTION('center_axis',(0.,0.,1.));
#11217=DIRECTION('ref_axis',(1.,0.,0.));
#11218=DIRECTION('center_axis',(0.,0.,1.));
#11219=DIRECTION('ref_axis',(1.,0.,0.));
#11220=DIRECTION('',(0.,0.,1.));
#11221=DIRECTION('center_axis',(0.,0.,-1.));
#11222=DIRECTION('ref_axis',(1.,0.,0.));
#11223=DIRECTION('center_axis',(0.,0.,1.));
#11224=DIRECTION('ref_axis',(1.,0.,0.));
#11225=DIRECTION('center_axis',(0.,0.,1.));
#11226=DIRECTION('ref_axis',(1.,0.,0.));
#11227=DIRECTION('',(0.,0.,1.));
#11228=DIRECTION('center_axis',(0.,0.,-1.));
#11229=DIRECTION('ref_axis',(1.,0.,0.));
#11230=DIRECTION('center_axis',(0.,0.,1.));
#11231=DIRECTION('ref_axis',(1.,0.,0.));
#11232=DIRECTION('center_axis',(0.,0.,1.));
#11233=DIRECTION('ref_axis',(1.,0.,0.));
#11234=DIRECTION('',(0.,0.,1.));
#11235=DIRECTION('center_axis',(0.,0.,-1.));
#11236=DIRECTION('ref_axis',(1.,0.,0.));
#11237=DIRECTION('center_axis',(0.,0.,1.));
#11238=DIRECTION('ref_axis',(1.,0.,0.));
#11239=DIRECTION('center_axis',(0.,0.,1.));
#11240=DIRECTION('ref_axis',(1.,0.,0.));
#11241=DIRECTION('',(0.,0.,1.));
#11242=DIRECTION('center_axis',(0.,0.,-1.));
#11243=DIRECTION('ref_axis',(1.,0.,0.));
#11244=DIRECTION('center_axis',(0.,0.,1.));
#11245=DIRECTION('ref_axis',(1.,0.,0.));
#11246=DIRECTION('center_axis',(0.,0.,1.));
#11247=DIRECTION('ref_axis',(1.,0.,0.));
#11248=DIRECTION('',(0.,0.,1.));
#11249=DIRECTION('center_axis',(0.,0.,-1.));
#11250=DIRECTION('ref_axis',(1.,0.,0.));
#11251=DIRECTION('center_axis',(0.,0.,1.));
#11252=DIRECTION('ref_axis',(1.,0.,0.));
#11253=DIRECTION('center_axis',(0.,0.,1.));
#11254=DIRECTION('ref_axis',(1.,0.,0.));
#11255=DIRECTION('',(0.,0.,1.));
#11256=DIRECTION('center_axis',(0.,0.,-1.));
#11257=DIRECTION('ref_axis',(1.,0.,0.));
#11258=DIRECTION('center_axis',(0.,0.,1.));
#11259=DIRECTION('ref_axis',(1.,0.,0.));
#11260=DIRECTION('center_axis',(0.,0.,1.));
#11261=DIRECTION('ref_axis',(1.,0.,0.));
#11262=DIRECTION('',(0.,0.,1.));
#11263=DIRECTION('center_axis',(0.,0.,-1.));
#11264=DIRECTION('ref_axis',(1.,0.,0.));
#11265=DIRECTION('center_axis',(0.,0.,1.));
#11266=DIRECTION('ref_axis',(1.,0.,0.));
#11267=DIRECTION('center_axis',(0.,0.,1.));
#11268=DIRECTION('ref_axis',(1.,0.,0.));
#11269=DIRECTION('',(0.,0.,1.));
#11270=DIRECTION('center_axis',(0.,0.,-1.));
#11271=DIRECTION('ref_axis',(1.,0.,0.));
#11272=DIRECTION('center_axis',(0.,0.,1.));
#11273=DIRECTION('ref_axis',(1.,0.,0.));
#11274=DIRECTION('center_axis',(0.,0.,1.));
#11275=DIRECTION('ref_axis',(1.,0.,0.));
#11276=DIRECTION('',(0.,0.,1.));
#11277=DIRECTION('center_axis',(0.,0.,-1.));
#11278=DIRECTION('ref_axis',(1.,0.,0.));
#11279=DIRECTION('center_axis',(0.,0.,1.));
#11280=DIRECTION('ref_axis',(1.,0.,0.));
#11281=DIRECTION('center_axis',(0.,0.,1.));
#11282=DIRECTION('ref_axis',(1.,0.,0.));
#11283=DIRECTION('',(0.,0.,1.));
#11284=DIRECTION('center_axis',(0.,0.,-1.));
#11285=DIRECTION('ref_axis',(1.,0.,0.));
#11286=DIRECTION('center_axis',(0.,0.,1.));
#11287=DIRECTION('ref_axis',(1.,0.,0.));
#11288=DIRECTION('center_axis',(0.,0.,1.));
#11289=DIRECTION('ref_axis',(1.,0.,0.));
#11290=DIRECTION('',(0.,0.,1.));
#11291=DIRECTION('center_axis',(0.,0.,-1.));
#11292=DIRECTION('ref_axis',(1.,0.,0.));
#11293=DIRECTION('center_axis',(0.,0.,1.));
#11294=DIRECTION('ref_axis',(1.,0.,0.));
#11295=DIRECTION('center_axis',(0.,0.,1.));
#11296=DIRECTION('ref_axis',(1.,0.,0.));
#11297=DIRECTION('',(0.,0.,1.));
#11298=DIRECTION('center_axis',(0.,0.,-1.));
#11299=DIRECTION('ref_axis',(1.,0.,0.));
#11300=DIRECTION('center_axis',(0.,0.,1.));
#11301=DIRECTION('ref_axis',(1.,0.,0.));
#11302=DIRECTION('center_axis',(0.,0.,1.));
#11303=DIRECTION('ref_axis',(1.,0.,0.));
#11304=DIRECTION('',(0.,0.,1.));
#11305=DIRECTION('center_axis',(0.,0.,-1.));
#11306=DIRECTION('ref_axis',(1.,0.,0.));
#11307=DIRECTION('center_axis',(0.,0.,1.));
#11308=DIRECTION('ref_axis',(1.,0.,0.));
#11309=DIRECTION('center_axis',(0.,0.,1.));
#11310=DIRECTION('ref_axis',(1.,0.,0.));
#11311=DIRECTION('',(0.,0.,1.));
#11312=DIRECTION('center_axis',(0.,0.,-1.));
#11313=DIRECTION('ref_axis',(1.,0.,0.));
#11314=DIRECTION('center_axis',(0.,1.,0.));
#11315=DIRECTION('ref_axis',(-1.,0.,0.));
#11316=DIRECTION('',(-1.,0.,0.));
#11317=DIRECTION('',(0.,0.,1.));
#11318=DIRECTION('',(-1.,0.,0.));
#11319=DIRECTION('',(0.,0.,1.));
#11320=DIRECTION('center_axis',(1.,0.,0.));
#11321=DIRECTION('ref_axis',(0.,1.,0.));
#11322=DIRECTION('',(0.,1.,0.));
#11323=DIRECTION('',(0.,1.,0.));
#11324=DIRECTION('',(0.,0.,1.));
#11325=DIRECTION('center_axis',(0.,-1.,0.));
#11326=DIRECTION('ref_axis',(1.,0.,0.));
#11327=DIRECTION('',(1.,0.,0.));
#11328=DIRECTION('',(1.,0.,0.));
#11329=DIRECTION('',(0.,0.,1.));
#11330=DIRECTION('center_axis',(-1.,0.,0.));
#11331=DIRECTION('ref_axis',(0.,-1.,0.));
#11332=DIRECTION('',(0.,-1.,0.));
#11333=DIRECTION('',(0.,-1.,0.));
#11334=DIRECTION('center_axis',(0.,0.,1.));
#11335=DIRECTION('ref_axis',(1.,0.,0.));
#11336=DIRECTION('center_axis',(0.,0.,1.));
#11337=DIRECTION('ref_axis',(1.,0.,0.));
#11338=DIRECTION('axis',(0.,0.,1.));
#11339=DIRECTION('refdir',(1.,0.,0.));
#11340=DIRECTION('center_axis',(0.,0.,1.));
#11341=DIRECTION('ref_axis',(1.,0.,0.));
#11342=DIRECTION('center_axis',(0.,0.,1.));
#11343=DIRECTION('ref_axis',(1.,0.,0.));
#11344=DIRECTION('',(0.,0.,1.));
#11345=DIRECTION('center_axis',(0.,0.,-1.));
#11346=DIRECTION('ref_axis',(1.,0.,0.));
#11347=DIRECTION('center_axis',(0.,0.,1.));
#11348=DIRECTION('ref_axis',(1.,0.,0.));
#11349=DIRECTION('center_axis',(0.,0.,1.));
#11350=DIRECTION('ref_axis',(1.,0.,0.));
#11351=DIRECTION('center_axis',(0.,0.,1.));
#11352=DIRECTION('ref_axis',(1.,0.,0.));
#11353=DIRECTION('',(0.,0.,1.));
#11354=DIRECTION('center_axis',(0.,0.,-1.));
#11355=DIRECTION('ref_axis',(1.,0.,0.));
#11356=DIRECTION('center_axis',(0.,0.,1.));
#11357=DIRECTION('ref_axis',(1.,0.,0.));
#11358=DIRECTION('center_axis',(0.,0.,1.));
#11359=DIRECTION('ref_axis',(1.,0.,0.));
#11360=DIRECTION('center_axis',(0.,0.,1.));
#11361=DIRECTION('ref_axis',(1.,0.,0.));
#11362=DIRECTION('',(0.,0.,1.));
#11363=DIRECTION('center_axis',(0.,0.,1.));
#11364=DIRECTION('ref_axis',(1.,0.,0.));
#11365=DIRECTION('center_axis',(0.,0.,1.));
#11366=DIRECTION('ref_axis',(1.,0.,0.));
#11367=DIRECTION('center_axis',(0.,0.,1.));
#11368=DIRECTION('ref_axis',(1.,0.,0.));
#11369=DIRECTION('center_axis',(0.,0.,1.));
#11370=DIRECTION('ref_axis',(1.,0.,0.));
#11371=DIRECTION('',(0.,0.,1.));
#11372=DIRECTION('center_axis',(0.,0.,1.));
#11373=DIRECTION('ref_axis',(1.,0.,0.));
#11374=DIRECTION('center_axis',(0.,0.,1.));
#11375=DIRECTION('ref_axis',(1.,0.,0.));
#11376=DIRECTION('center_axis',(0.,1.,0.));
#11377=DIRECTION('ref_axis',(-1.,0.,0.));
#11378=DIRECTION('',(-1.,0.,0.));
#11379=DIRECTION('',(0.,0.,1.));
#11380=DIRECTION('',(-1.,0.,0.));
#11381=DIRECTION('',(0.,0.,1.));
#11382=DIRECTION('center_axis',(1.,0.,0.));
#11383=DIRECTION('ref_axis',(0.,1.,0.));
#11384=DIRECTION('',(0.,1.,0.));
#11385=DIRECTION('',(0.,1.,0.));
#11386=DIRECTION('',(0.,0.,1.));
#11387=DIRECTION('center_axis',(0.,-1.,0.));
#11388=DIRECTION('ref_axis',(1.,0.,0.));
#11389=DIRECTION('',(1.,0.,0.));
#11390=DIRECTION('',(1.,0.,0.));
#11391=DIRECTION('',(0.,0.,1.));
#11392=DIRECTION('center_axis',(-1.,0.,0.));
#11393=DIRECTION('ref_axis',(0.,-1.,0.));
#11394=DIRECTION('',(0.,-1.,0.));
#11395=DIRECTION('',(0.,-1.,0.));
#11396=DIRECTION('center_axis',(0.,0.,1.));
#11397=DIRECTION('ref_axis',(1.,0.,0.));
#11398=DIRECTION('center_axis',(0.,0.,1.));
#11399=DIRECTION('ref_axis',(1.,0.,0.));
#11400=DIRECTION('axis',(0.,0.,1.));
#11401=DIRECTION('refdir',(1.,0.,0.));
#11402=DIRECTION('center_axis',(0.,0.,1.));
#11403=DIRECTION('ref_axis',(1.,0.,0.));
#11404=DIRECTION('center_axis',(0.,0.,1.));
#11405=DIRECTION('ref_axis',(1.,0.,0.));
#11406=DIRECTION('',(0.,0.,1.));
#11407=DIRECTION('center_axis',(0.,0.,-1.));
#11408=DIRECTION('ref_axis',(1.,0.,0.));
#11409=DIRECTION('center_axis',(0.,0.,1.));
#11410=DIRECTION('ref_axis',(1.,0.,0.));
#11411=DIRECTION('center_axis',(0.,0.,1.));
#11412=DIRECTION('ref_axis',(1.,0.,0.));
#11413=DIRECTION('center_axis',(0.,0.,1.));
#11414=DIRECTION('ref_axis',(1.,0.,0.));
#11415=DIRECTION('',(0.,0.,1.));
#11416=DIRECTION('center_axis',(0.,0.,-1.));
#11417=DIRECTION('ref_axis',(1.,0.,0.));
#11418=DIRECTION('center_axis',(0.,0.,1.));
#11419=DIRECTION('ref_axis',(1.,0.,0.));
#11420=DIRECTION('center_axis',(0.,0.,1.));
#11421=DIRECTION('ref_axis',(1.,0.,0.));
#11422=DIRECTION('center_axis',(0.,0.,1.));
#11423=DIRECTION('ref_axis',(1.,0.,0.));
#11424=DIRECTION('',(0.,0.,1.));
#11425=DIRECTION('center_axis',(0.,0.,1.));
#11426=DIRECTION('ref_axis',(1.,0.,0.));
#11427=DIRECTION('center_axis',(0.,0.,1.));
#11428=DIRECTION('ref_axis',(1.,0.,0.));
#11429=DIRECTION('center_axis',(0.,0.,1.));
#11430=DIRECTION('ref_axis',(1.,0.,0.));
#11431=DIRECTION('center_axis',(0.,0.,1.));
#11432=DIRECTION('ref_axis',(1.,0.,0.));
#11433=DIRECTION('',(0.,0.,1.));
#11434=DIRECTION('center_axis',(0.,0.,1.));
#11435=DIRECTION('ref_axis',(1.,0.,0.));
#11436=DIRECTION('center_axis',(0.,0.,1.));
#11437=DIRECTION('ref_axis',(1.,0.,0.));
#11438=DIRECTION('center_axis',(0.,1.,0.));
#11439=DIRECTION('ref_axis',(-1.,0.,0.));
#11440=DIRECTION('',(-1.,0.,0.));
#11441=DIRECTION('',(0.,0.,1.));
#11442=DIRECTION('',(-1.,0.,0.));
#11443=DIRECTION('',(0.,0.,1.));
#11444=DIRECTION('center_axis',(1.,0.,0.));
#11445=DIRECTION('ref_axis',(0.,1.,0.));
#11446=DIRECTION('',(0.,1.,0.));
#11447=DIRECTION('',(0.,1.,0.));
#11448=DIRECTION('',(0.,0.,1.));
#11449=DIRECTION('center_axis',(0.,-1.,0.));
#11450=DIRECTION('ref_axis',(1.,0.,0.));
#11451=DIRECTION('',(1.,0.,0.));
#11452=DIRECTION('',(1.,0.,0.));
#11453=DIRECTION('',(0.,0.,1.));
#11454=DIRECTION('center_axis',(-1.,0.,0.));
#11455=DIRECTION('ref_axis',(0.,-1.,0.));
#11456=DIRECTION('',(0.,-1.,0.));
#11457=DIRECTION('',(0.,-1.,0.));
#11458=DIRECTION('center_axis',(0.,0.,1.));
#11459=DIRECTION('ref_axis',(1.,0.,0.));
#11460=DIRECTION('center_axis',(0.,0.,1.));
#11461=DIRECTION('ref_axis',(1.,0.,0.));
#11462=DIRECTION('axis',(0.,0.,1.));
#11463=DIRECTION('refdir',(1.,0.,0.));
#11464=DIRECTION('center_axis',(0.,0.,1.));
#11465=DIRECTION('ref_axis',(1.,0.,0.));
#11466=DIRECTION('center_axis',(0.,0.,1.));
#11467=DIRECTION('ref_axis',(1.,0.,0.));
#11468=DIRECTION('',(0.,0.,1.));
#11469=DIRECTION('center_axis',(0.,0.,1.));
#11470=DIRECTION('ref_axis',(1.,0.,0.));
#11471=DIRECTION('center_axis',(0.,0.,1.));
#11472=DIRECTION('ref_axis',(1.,0.,0.));
#11473=DIRECTION('center_axis',(0.,0.,1.));
#11474=DIRECTION('ref_axis',(1.,0.,0.));
#11475=DIRECTION('center_axis',(0.,0.,1.));
#11476=DIRECTION('ref_axis',(1.,0.,0.));
#11477=DIRECTION('',(0.,0.,1.));
#11478=DIRECTION('center_axis',(0.,0.,1.));
#11479=DIRECTION('ref_axis',(1.,0.,0.));
#11480=DIRECTION('center_axis',(0.,0.,1.));
#11481=DIRECTION('ref_axis',(1.,0.,0.));
#11482=DIRECTION('center_axis',(0.,1.,0.));
#11483=DIRECTION('ref_axis',(1.,0.,0.));
#11484=DIRECTION('center_axis',(0.,1.,0.));
#11485=DIRECTION('ref_axis',(1.,0.,0.));
#11486=DIRECTION('',(0.,1.,0.));
#11487=DIRECTION('center_axis',(0.,-1.,0.));
#11488=DIRECTION('ref_axis',(1.,0.,0.));
#11489=DIRECTION('center_axis',(0.,1.,0.));
#11490=DIRECTION('ref_axis',(1.,0.,0.));
#11491=DIRECTION('center_axis',(0.,1.,0.));
#11492=DIRECTION('ref_axis',(1.,0.,0.));
#11493=DIRECTION('',(0.,1.,0.));
#11494=DIRECTION('center_axis',(0.,-1.,0.));
#11495=DIRECTION('ref_axis',(1.,0.,0.));
#11496=DIRECTION('center_axis',(0.,1.,0.));
#11497=DIRECTION('ref_axis',(-1.,0.,0.));
#11498=DIRECTION('',(-1.,0.,0.));
#11499=DIRECTION('',(0.,0.,1.));
#11500=DIRECTION('',(-1.,0.,0.));
#11501=DIRECTION('',(0.,0.,1.));
#11502=DIRECTION('center_axis',(1.,0.,0.));
#11503=DIRECTION('ref_axis',(0.,1.,0.));
#11504=DIRECTION('',(0.,1.,0.));
#11505=DIRECTION('',(0.,1.,0.));
#11506=DIRECTION('',(0.,0.,1.));
#11507=DIRECTION('center_axis',(0.,-1.,0.));
#11508=DIRECTION('ref_axis',(1.,0.,0.));
#11509=DIRECTION('',(1.,0.,0.));
#11510=DIRECTION('',(1.,0.,0.));
#11511=DIRECTION('',(0.,0.,1.));
#11512=DIRECTION('center_axis',(-1.,0.,0.));
#11513=DIRECTION('ref_axis',(0.,-1.,0.));
#11514=DIRECTION('',(0.,-1.,0.));
#11515=DIRECTION('',(0.,-1.,0.));
#11516=DIRECTION('center_axis',(0.,0.,1.));
#11517=DIRECTION('ref_axis',(1.,0.,0.));
#11518=DIRECTION('center_axis',(0.,0.,1.));
#11519=DIRECTION('ref_axis',(1.,0.,0.));
#11520=DIRECTION('axis',(0.,0.,1.));
#11521=DIRECTION('refdir',(1.,0.,0.));
#11522=DIRECTION('center_axis',(0.,0.,1.));
#11523=DIRECTION('ref_axis',(1.,0.,0.));
#11524=DIRECTION('center_axis',(0.,0.,1.));
#11525=DIRECTION('ref_axis',(1.,0.,0.));
#11526=DIRECTION('',(0.,0.,1.));
#11527=DIRECTION('center_axis',(0.,0.,-1.));
#11528=DIRECTION('ref_axis',(1.,0.,0.));
#11529=DIRECTION('center_axis',(0.,0.,1.));
#11530=DIRECTION('ref_axis',(1.,0.,0.));
#11531=DIRECTION('center_axis',(0.,0.,1.));
#11532=DIRECTION('ref_axis',(1.,0.,0.));
#11533=DIRECTION('',(0.,0.,1.));
#11534=DIRECTION('center_axis',(0.,0.,-1.));
#11535=DIRECTION('ref_axis',(1.,0.,0.));
#11536=DIRECTION('center_axis',(0.,1.,0.));
#11537=DIRECTION('ref_axis',(1.,0.,0.));
#11538=DIRECTION('center_axis',(0.,1.,0.));
#11539=DIRECTION('ref_axis',(1.,0.,0.));
#11540=DIRECTION('',(0.,1.,0.));
#11541=DIRECTION('center_axis',(0.,1.,0.));
#11542=DIRECTION('ref_axis',(1.,0.,0.));
#11543=DIRECTION('',(0.,1.,0.));
#11544=DIRECTION('center_axis',(0.,-1.,0.));
#11545=DIRECTION('ref_axis',(1.,0.,0.));
#11546=DIRECTION('',(0.,-1.,0.));
#11547=DIRECTION('center_axis',(0.,1.,0.));
#11548=DIRECTION('ref_axis',(1.,0.,0.));
#11549=DIRECTION('center_axis',(0.,1.,0.));
#11550=DIRECTION('ref_axis',(1.,0.,0.));
#11551=DIRECTION('',(-1.,0.,0.));
#11552=DIRECTION('center_axis',(0.,1.,0.));
#11553=DIRECTION('ref_axis',(1.,0.,0.));
#11554=DIRECTION('center_axis',(0.,1.,0.));
#11555=DIRECTION('ref_axis',(1.,0.,0.));
#11556=DIRECTION('',(0.,1.,0.));
#11557=DIRECTION('center_axis',(0.,1.,0.));
#11558=DIRECTION('ref_axis',(1.,0.,0.));
#11559=DIRECTION('',(0.,1.,0.));
#11560=DIRECTION('center_axis',(0.,-1.,0.));
#11561=DIRECTION('ref_axis',(1.,0.,0.));
#11562=DIRECTION('',(0.,-1.,0.));
#11563=DIRECTION('center_axis',(0.,1.,0.));
#11564=DIRECTION('ref_axis',(1.,0.,0.));
#11565=DIRECTION('center_axis',(0.,1.,0.));
#11566=DIRECTION('ref_axis',(1.,0.,0.));
#11567=DIRECTION('',(-1.,0.,0.));
#11568=DIRECTION('center_axis',(0.,1.,0.));
#11569=DIRECTION('ref_axis',(-1.,0.,0.));
#11570=DIRECTION('',(1.,0.,0.));
#11571=DIRECTION('',(1.,0.,0.));
#11572=DIRECTION('',(0.,0.,1.));
#11573=DIRECTION('',(-1.,0.,0.));
#11574=DIRECTION('',(0.,0.,1.));
#11575=DIRECTION('',(1.,0.,0.));
#11576=DIRECTION('center_axis',(0.,0.,-1.));
#11577=DIRECTION('ref_axis',(-1.,0.,0.));
#11578=DIRECTION('',(0.,1.,0.));
#11579=DIRECTION('',(-1.,0.,0.));
#11580=DIRECTION('',(0.,1.,0.));
#11581=DIRECTION('center_axis',(0.,1.,0.));
#11582=DIRECTION('ref_axis',(0.,0.,1.));
#11583=DIRECTION('',(1.,0.,0.));
#11584=DIRECTION('',(0.,0.,-1.));
#11585=DIRECTION('',(0.,0.,1.));
#11586=DIRECTION('center_axis',(1.,0.,0.));
#11587=DIRECTION('ref_axis',(0.,1.,0.));
#11588=DIRECTION('',(0.,0.,1.));
#11589=DIRECTION('',(0.,1.,0.));
#11590=DIRECTION('',(0.,1.,0.));
#11591=DIRECTION('center_axis',(0.,-1.,0.));
#11592=DIRECTION('ref_axis',(1.,0.,0.));
#11593=DIRECTION('',(0.,0.,1.));
#11594=DIRECTION('',(1.,0.,0.));
#11595=DIRECTION('',(1.,0.,0.));
#11596=DIRECTION('center_axis',(-1.,0.,0.));
#11597=DIRECTION('ref_axis',(0.,-1.,0.));
#11598=DIRECTION('',(0.,-1.,0.));
#11599=DIRECTION('',(0.,1.,0.));
#11600=DIRECTION('center_axis',(0.,0.,1.));
#11601=DIRECTION('ref_axis',(1.,0.,0.));
#11602=DIRECTION('center_axis',(0.,0.,1.));
#11603=DIRECTION('ref_axis',(1.,0.,0.));
#11604=DIRECTION('axis',(0.,0.,1.));
#11605=DIRECTION('refdir',(1.,0.,0.));
#11606=DIRECTION('center_axis',(0.,0.,1.));
#11607=DIRECTION('ref_axis',(1.,0.,0.));
#11608=DIRECTION('center_axis',(0.,0.,-1.));
#11609=DIRECTION('ref_axis',(1.,0.,0.));
#11610=DIRECTION('',(0.,0.,-1.));
#11611=DIRECTION('center_axis',(0.,0.,-1.));
#11612=DIRECTION('ref_axis',(1.,0.,0.));
#11613=DIRECTION('center_axis',(0.,0.,1.));
#11614=DIRECTION('ref_axis',(1.,0.,0.));
#11615=DIRECTION('center_axis',(0.,0.,1.));
#11616=DIRECTION('ref_axis',(1.,0.,0.));
#11617=DIRECTION('',(0.,0.,-1.));
#11618=DIRECTION('center_axis',(0.,0.,1.));
#11619=DIRECTION('ref_axis',(1.,0.,0.));
#11620=DIRECTION('center_axis',(0.,0.,1.));
#11621=DIRECTION('ref_axis',(1.,0.,0.));
#11622=DIRECTION('center_axis',(0.,0.,1.));
#11623=DIRECTION('ref_axis',(1.,0.,0.));
#11624=DIRECTION('axis',(0.,0.,1.));
#11625=DIRECTION('refdir',(1.,0.,0.));
#11626=DIRECTION('center_axis',(-0.000133356290274077,0.990604928518996,
0.136754735969086));
#11627=DIRECTION('ref_axis',(1.84100680060121E-5,-0.136754734729895,0.990604937495279));
#11628=DIRECTION('center_axis',(0.000133356194773129,0.99060492849245,0.136754736161472));
#11629=DIRECTION('ref_axis',(-0.722226697925938,0.0946826990450871,-0.685145081938514));
#11630=DIRECTION('center_axis',(0.000133356194773129,0.99060492849245,0.136754736161472));
#11631=DIRECTION('ref_axis',(-0.722226697925938,0.0946826990450871,-0.685145081938514));
#11632=DIRECTION('center_axis',(-0.000133356290274077,0.990604928518996,
0.136754735969086));
#11633=DIRECTION('ref_axis',(1.84100680060121E-5,-0.136754734729895,0.990604937495279));
#11634=DIRECTION('axis',(0.,0.,1.));
#11635=DIRECTION('refdir',(1.,0.,0.));
#11636=DIRECTION('center_axis',(0.,0.,1.));
#11637=DIRECTION('ref_axis',(1.,0.,0.));
#11638=DIRECTION('center_axis',(0.,0.,1.));
#11639=DIRECTION('ref_axis',(1.,0.,0.));
#11640=DIRECTION('',(0.,0.,1.));
#11641=DIRECTION('center_axis',(0.,0.,1.));
#11642=DIRECTION('ref_axis',(1.,0.,0.));
#11643=DIRECTION('center_axis',(0.,0.,1.));
#11644=DIRECTION('ref_axis',(1.,0.,0.));
#11645=DIRECTION('center_axis',(0.,0.,1.));
#11646=DIRECTION('ref_axis',(1.,0.,0.));
#11647=DIRECTION('center_axis',(0.,0.,1.));
#11648=DIRECTION('ref_axis',(1.,0.,0.));
#11649=DIRECTION('',(0.,0.,1.));
#11650=DIRECTION('center_axis',(0.,0.,1.));
#11651=DIRECTION('ref_axis',(1.,0.,0.));
#11652=DIRECTION('center_axis',(0.,0.,1.));
#11653=DIRECTION('ref_axis',(1.,0.,0.));
#11654=DIRECTION('center_axis',(0.,1.,0.));
#11655=DIRECTION('ref_axis',(1.,0.,0.));
#11656=DIRECTION('center_axis',(0.,1.,0.));
#11657=DIRECTION('ref_axis',(1.,0.,0.));
#11658=DIRECTION('',(0.,1.,0.));
#11659=DIRECTION('center_axis',(0.,-1.,0.));
#11660=DIRECTION('ref_axis',(1.,0.,0.));
#11661=DIRECTION('center_axis',(0.,1.,0.));
#11662=DIRECTION('ref_axis',(1.,0.,0.));
#11663=DIRECTION('center_axis',(0.,1.,0.));
#11664=DIRECTION('ref_axis',(1.,0.,0.));
#11665=DIRECTION('',(0.,1.,0.));
#11666=DIRECTION('center_axis',(0.,-1.,0.));
#11667=DIRECTION('ref_axis',(1.,0.,0.));
#11668=DIRECTION('center_axis',(0.,1.,0.));
#11669=DIRECTION('ref_axis',(-1.,0.,0.));
#11670=DIRECTION('',(-1.,0.,0.));
#11671=DIRECTION('',(0.,0.,1.));
#11672=DIRECTION('',(-1.,0.,0.));
#11673=DIRECTION('',(0.,0.,1.));
#11674=DIRECTION('center_axis',(1.,0.,0.));
#11675=DIRECTION('ref_axis',(0.,1.,0.));
#11676=DIRECTION('',(0.,1.,0.));
#11677=DIRECTION('',(0.,1.,0.));
#11678=DIRECTION('',(0.,0.,1.));
#11679=DIRECTION('center_axis',(0.,-1.,0.));
#11680=DIRECTION('ref_axis',(1.,0.,0.));
#11681=DIRECTION('',(1.,0.,0.));
#11682=DIRECTION('',(1.,0.,0.));
#11683=DIRECTION('',(0.,0.,1.));
#11684=DIRECTION('center_axis',(-1.,0.,0.));
#11685=DIRECTION('ref_axis',(0.,-1.,0.));
#11686=DIRECTION('',(0.,-1.,0.));
#11687=DIRECTION('',(0.,-1.,0.));
#11688=DIRECTION('center_axis',(0.,0.,1.));
#11689=DIRECTION('ref_axis',(1.,0.,0.));
#11690=DIRECTION('center_axis',(0.,0.,1.));
#11691=DIRECTION('ref_axis',(1.,0.,0.));
#11692=DIRECTION('axis',(0.,0.,1.));
#11693=DIRECTION('refdir',(1.,0.,0.));
#11694=DIRECTION('center_axis',(0.,0.,1.));
#11695=DIRECTION('ref_axis',(1.,0.,0.));
#11696=DIRECTION('center_axis',(0.,0.,1.));
#11697=DIRECTION('ref_axis',(1.,0.,0.));
#11698=DIRECTION('',(0.,0.,1.));
#11699=DIRECTION('center_axis',(0.,0.,-1.));
#11700=DIRECTION('ref_axis',(1.,0.,0.));
#11701=DIRECTION('center_axis',(0.,0.,1.));
#11702=DIRECTION('ref_axis',(1.,0.,0.));
#11703=DIRECTION('center_axis',(0.,0.,1.));
#11704=DIRECTION('ref_axis',(1.,0.,0.));
#11705=DIRECTION('',(0.,0.,1.));
#11706=DIRECTION('center_axis',(0.,0.,-1.));
#11707=DIRECTION('ref_axis',(1.,0.,0.));
#11708=DIRECTION('center_axis',(0.,1.,0.));
#11709=DIRECTION('ref_axis',(1.,0.,0.));
#11710=DIRECTION('center_axis',(0.,1.,0.));
#11711=DIRECTION('ref_axis',(1.,0.,0.));
#11712=DIRECTION('',(0.,1.,0.));
#11713=DIRECTION('center_axis',(0.,1.,0.));
#11714=DIRECTION('ref_axis',(1.,0.,0.));
#11715=DIRECTION('',(0.,1.,0.));
#11716=DIRECTION('center_axis',(0.,-1.,0.));
#11717=DIRECTION('ref_axis',(1.,0.,0.));
#11718=DIRECTION('',(0.,-1.,0.));
#11719=DIRECTION('center_axis',(0.,1.,0.));
#11720=DIRECTION('ref_axis',(1.,0.,0.));
#11721=DIRECTION('center_axis',(0.,1.,0.));
#11722=DIRECTION('ref_axis',(1.,0.,0.));
#11723=DIRECTION('',(-1.,0.,0.));
#11724=DIRECTION('center_axis',(0.,1.,0.));
#11725=DIRECTION('ref_axis',(1.,0.,0.));
#11726=DIRECTION('center_axis',(0.,1.,0.));
#11727=DIRECTION('ref_axis',(1.,0.,0.));
#11728=DIRECTION('',(0.,1.,0.));
#11729=DIRECTION('center_axis',(0.,1.,0.));
#11730=DIRECTION('ref_axis',(1.,0.,0.));
#11731=DIRECTION('',(0.,1.,0.));
#11732=DIRECTION('center_axis',(0.,-1.,0.));
#11733=DIRECTION('ref_axis',(1.,0.,0.));
#11734=DIRECTION('',(0.,-1.,0.));
#11735=DIRECTION('center_axis',(0.,1.,0.));
#11736=DIRECTION('ref_axis',(1.,0.,0.));
#11737=DIRECTION('center_axis',(0.,1.,0.));
#11738=DIRECTION('ref_axis',(1.,0.,0.));
#11739=DIRECTION('',(-1.,0.,0.));
#11740=DIRECTION('center_axis',(0.,1.,0.));
#11741=DIRECTION('ref_axis',(-1.,0.,0.));
#11742=DIRECTION('',(1.,0.,0.));
#11743=DIRECTION('',(1.,0.,0.));
#11744=DIRECTION('',(0.,0.,1.));
#11745=DIRECTION('',(-1.,0.,0.));
#11746=DIRECTION('',(0.,0.,1.));
#11747=DIRECTION('',(1.,0.,0.));
#11748=DIRECTION('center_axis',(0.,0.,-1.));
#11749=DIRECTION('ref_axis',(-1.,0.,0.));
#11750=DIRECTION('',(0.,1.,0.));
#11751=DIRECTION('',(-1.,0.,0.));
#11752=DIRECTION('',(0.,1.,0.));
#11753=DIRECTION('center_axis',(0.,1.,0.));
#11754=DIRECTION('ref_axis',(0.,0.,1.));
#11755=DIRECTION('',(1.,0.,0.));
#11756=DIRECTION('',(0.,0.,-1.));
#11757=DIRECTION('',(0.,0.,1.));
#11758=DIRECTION('center_axis',(1.,0.,0.));
#11759=DIRECTION('ref_axis',(0.,1.,0.));
#11760=DIRECTION('',(0.,0.,1.));
#11761=DIRECTION('',(0.,1.,0.));
#11762=DIRECTION('',(0.,1.,0.));
#11763=DIRECTION('center_axis',(0.,-1.,0.));
#11764=DIRECTION('ref_axis',(1.,0.,0.));
#11765=DIRECTION('',(0.,0.,1.));
#11766=DIRECTION('',(1.,0.,0.));
#11767=DIRECTION('',(1.,0.,0.));
#11768=DIRECTION('center_axis',(-1.,0.,0.));
#11769=DIRECTION('ref_axis',(0.,-1.,0.));
#11770=DIRECTION('',(0.,-1.,0.));
#11771=DIRECTION('',(0.,1.,0.));
#11772=DIRECTION('center_axis',(0.,0.,1.));
#11773=DIRECTION('ref_axis',(1.,0.,0.));
#11774=DIRECTION('center_axis',(0.,0.,1.));
#11775=DIRECTION('ref_axis',(1.,0.,0.));
#11776=DIRECTION('axis',(0.,0.,1.));
#11777=DIRECTION('refdir',(1.,0.,0.));
#11778=DIRECTION('center_axis',(0.,0.,1.));
#11779=DIRECTION('ref_axis',(1.,0.,0.));
#11780=DIRECTION('center_axis',(0.,0.,-1.));
#11781=DIRECTION('ref_axis',(1.,0.,0.));
#11782=DIRECTION('',(0.,0.,-1.));
#11783=DIRECTION('center_axis',(0.,0.,-1.));
#11784=DIRECTION('ref_axis',(1.,0.,0.));
#11785=DIRECTION('center_axis',(0.,0.,1.));
#11786=DIRECTION('ref_axis',(1.,0.,0.));
#11787=DIRECTION('center_axis',(0.,0.,1.));
#11788=DIRECTION('ref_axis',(1.,0.,0.));
#11789=DIRECTION('',(0.,0.,-1.));
#11790=DIRECTION('center_axis',(0.,0.,1.));
#11791=DIRECTION('ref_axis',(1.,0.,0.));
#11792=DIRECTION('center_axis',(0.,0.,1.));
#11793=DIRECTION('ref_axis',(1.,0.,0.));
#11794=DIRECTION('center_axis',(0.,0.,1.));
#11795=DIRECTION('ref_axis',(1.,0.,0.));
#11796=DIRECTION('axis',(0.,0.,1.));
#11797=DIRECTION('refdir',(1.,0.,0.));
#11798=DIRECTION('center_axis',(-0.000133356290794322,0.990604928516086,
0.136754735990165));
#11799=DIRECTION('ref_axis',(1.84100680806489E-5,-0.136754734750974,0.990604937492369));
#11800=DIRECTION('center_axis',(0.000133356202123069,0.990604928495684,
0.13675473613804));
#11801=DIRECTION('ref_axis',(-0.722226697925981,0.0946826990341326,-0.685145081939983));
#11802=DIRECTION('center_axis',(0.000133356202123069,0.990604928495684,
0.13675473613804));
#11803=DIRECTION('ref_axis',(-0.722226697925981,0.0946826990341325,-0.685145081939983));
#11804=DIRECTION('center_axis',(-0.000133356290794322,0.990604928516086,
0.136754735990165));
#11805=DIRECTION('ref_axis',(1.84100680806489E-5,-0.136754734750974,0.990604937492369));
#11806=DIRECTION('axis',(0.,0.,1.));
#11807=DIRECTION('refdir',(1.,0.,0.));
#11808=DIRECTION('center_axis',(0.,0.,1.));
#11809=DIRECTION('ref_axis',(1.,0.,0.));
#11810=DIRECTION('center_axis',(0.,0.,1.));
#11811=DIRECTION('ref_axis',(1.,0.,0.));
#11812=DIRECTION('',(0.,0.,1.));
#11813=DIRECTION('center_axis',(0.,0.,1.));
#11814=DIRECTION('ref_axis',(1.,0.,0.));
#11815=DIRECTION('center_axis',(0.,0.,1.));
#11816=DIRECTION('ref_axis',(1.,0.,0.));
#11817=DIRECTION('center_axis',(0.,0.,1.));
#11818=DIRECTION('ref_axis',(1.,0.,0.));
#11819=DIRECTION('center_axis',(0.,0.,1.));
#11820=DIRECTION('ref_axis',(1.,0.,0.));
#11821=DIRECTION('',(0.,0.,1.));
#11822=DIRECTION('center_axis',(0.,0.,1.));
#11823=DIRECTION('ref_axis',(1.,0.,0.));
#11824=DIRECTION('center_axis',(0.,0.,1.));
#11825=DIRECTION('ref_axis',(1.,0.,0.));
#11826=DIRECTION('center_axis',(0.,1.,0.));
#11827=DIRECTION('ref_axis',(1.,0.,0.));
#11828=DIRECTION('center_axis',(0.,1.,0.));
#11829=DIRECTION('ref_axis',(1.,0.,0.));
#11830=DIRECTION('',(0.,1.,0.));
#11831=DIRECTION('center_axis',(0.,-1.,0.));
#11832=DIRECTION('ref_axis',(1.,0.,0.));
#11833=DIRECTION('center_axis',(0.,1.,0.));
#11834=DIRECTION('ref_axis',(1.,0.,0.));
#11835=DIRECTION('center_axis',(0.,1.,0.));
#11836=DIRECTION('ref_axis',(1.,0.,0.));
#11837=DIRECTION('',(0.,1.,0.));
#11838=DIRECTION('center_axis',(0.,-1.,0.));
#11839=DIRECTION('ref_axis',(1.,0.,0.));
#11840=DIRECTION('center_axis',(0.,1.,0.));
#11841=DIRECTION('ref_axis',(-1.,0.,0.));
#11842=DIRECTION('',(-1.,0.,0.));
#11843=DIRECTION('',(0.,0.,1.));
#11844=DIRECTION('',(-1.,0.,0.));
#11845=DIRECTION('',(0.,0.,1.));
#11846=DIRECTION('center_axis',(1.,0.,0.));
#11847=DIRECTION('ref_axis',(0.,1.,0.));
#11848=DIRECTION('',(0.,1.,0.));
#11849=DIRECTION('',(0.,1.,0.));
#11850=DIRECTION('',(0.,0.,1.));
#11851=DIRECTION('center_axis',(0.,-1.,0.));
#11852=DIRECTION('ref_axis',(1.,0.,0.));
#11853=DIRECTION('',(1.,0.,0.));
#11854=DIRECTION('',(1.,0.,0.));
#11855=DIRECTION('',(0.,0.,1.));
#11856=DIRECTION('center_axis',(-1.,0.,0.));
#11857=DIRECTION('ref_axis',(0.,-1.,0.));
#11858=DIRECTION('',(0.,-1.,0.));
#11859=DIRECTION('',(0.,-1.,0.));
#11860=DIRECTION('center_axis',(0.,0.,1.));
#11861=DIRECTION('ref_axis',(1.,0.,0.));
#11862=DIRECTION('center_axis',(0.,0.,1.));
#11863=DIRECTION('ref_axis',(1.,0.,0.));
#11864=DIRECTION('axis',(0.,0.,1.));
#11865=DIRECTION('refdir',(1.,0.,0.));
#11866=DIRECTION('center_axis',(0.,0.,1.));
#11867=DIRECTION('ref_axis',(1.,0.,0.));
#11868=DIRECTION('center_axis',(0.,0.,1.));
#11869=DIRECTION('ref_axis',(1.,0.,0.));
#11870=DIRECTION('',(0.,0.,1.));
#11871=DIRECTION('center_axis',(0.,0.,-1.));
#11872=DIRECTION('ref_axis',(1.,0.,0.));
#11873=DIRECTION('center_axis',(0.,0.,1.));
#11874=DIRECTION('ref_axis',(1.,0.,0.));
#11875=DIRECTION('center_axis',(0.,0.,1.));
#11876=DIRECTION('ref_axis',(1.,0.,0.));
#11877=DIRECTION('',(0.,0.,1.));
#11878=DIRECTION('center_axis',(0.,0.,-1.));
#11879=DIRECTION('ref_axis',(1.,0.,0.));
#11880=DIRECTION('center_axis',(0.,1.,0.));
#11881=DIRECTION('ref_axis',(1.,0.,0.));
#11882=DIRECTION('center_axis',(0.,1.,0.));
#11883=DIRECTION('ref_axis',(1.,0.,0.));
#11884=DIRECTION('',(0.,1.,0.));
#11885=DIRECTION('center_axis',(0.,1.,0.));
#11886=DIRECTION('ref_axis',(1.,0.,0.));
#11887=DIRECTION('',(0.,1.,0.));
#11888=DIRECTION('center_axis',(0.,-1.,0.));
#11889=DIRECTION('ref_axis',(1.,0.,0.));
#11890=DIRECTION('',(0.,-1.,0.));
#11891=DIRECTION('center_axis',(0.,1.,0.));
#11892=DIRECTION('ref_axis',(1.,0.,0.));
#11893=DIRECTION('center_axis',(0.,1.,0.));
#11894=DIRECTION('ref_axis',(1.,0.,0.));
#11895=DIRECTION('',(-1.,0.,0.));
#11896=DIRECTION('center_axis',(0.,1.,0.));
#11897=DIRECTION('ref_axis',(1.,0.,0.));
#11898=DIRECTION('center_axis',(0.,1.,0.));
#11899=DIRECTION('ref_axis',(1.,0.,0.));
#11900=DIRECTION('',(0.,1.,0.));
#11901=DIRECTION('center_axis',(0.,1.,0.));
#11902=DIRECTION('ref_axis',(1.,0.,0.));
#11903=DIRECTION('',(0.,1.,0.));
#11904=DIRECTION('center_axis',(0.,-1.,0.));
#11905=DIRECTION('ref_axis',(1.,0.,0.));
#11906=DIRECTION('',(0.,-1.,0.));
#11907=DIRECTION('center_axis',(0.,1.,0.));
#11908=DIRECTION('ref_axis',(1.,0.,0.));
#11909=DIRECTION('center_axis',(0.,1.,0.));
#11910=DIRECTION('ref_axis',(1.,0.,0.));
#11911=DIRECTION('',(-1.,0.,0.));
#11912=DIRECTION('center_axis',(0.,1.,0.));
#11913=DIRECTION('ref_axis',(-1.,0.,0.));
#11914=DIRECTION('',(1.,0.,0.));
#11915=DIRECTION('',(1.,0.,0.));
#11916=DIRECTION('',(0.,0.,1.));
#11917=DIRECTION('',(-1.,0.,0.));
#11918=DIRECTION('',(0.,0.,1.));
#11919=DIRECTION('',(1.,0.,0.));
#11920=DIRECTION('center_axis',(0.,0.,-1.));
#11921=DIRECTION('ref_axis',(-1.,0.,0.));
#11922=DIRECTION('',(0.,1.,0.));
#11923=DIRECTION('',(-1.,0.,0.));
#11924=DIRECTION('',(0.,1.,0.));
#11925=DIRECTION('center_axis',(0.,1.,0.));
#11926=DIRECTION('ref_axis',(0.,0.,1.));
#11927=DIRECTION('',(1.,0.,0.));
#11928=DIRECTION('',(0.,0.,-1.));
#11929=DIRECTION('',(0.,0.,1.));
#11930=DIRECTION('center_axis',(1.,0.,0.));
#11931=DIRECTION('ref_axis',(0.,1.,0.));
#11932=DIRECTION('',(0.,0.,1.));
#11933=DIRECTION('',(0.,1.,0.));
#11934=DIRECTION('',(0.,1.,0.));
#11935=DIRECTION('center_axis',(0.,-1.,0.));
#11936=DIRECTION('ref_axis',(1.,0.,0.));
#11937=DIRECTION('',(0.,0.,1.));
#11938=DIRECTION('',(1.,0.,0.));
#11939=DIRECTION('',(1.,0.,0.));
#11940=DIRECTION('center_axis',(-1.,0.,0.));
#11941=DIRECTION('ref_axis',(0.,-1.,0.));
#11942=DIRECTION('',(0.,-1.,0.));
#11943=DIRECTION('',(0.,1.,0.));
#11944=DIRECTION('center_axis',(0.,0.,1.));
#11945=DIRECTION('ref_axis',(1.,0.,0.));
#11946=DIRECTION('center_axis',(0.,0.,1.));
#11947=DIRECTION('ref_axis',(1.,0.,0.));
#11948=DIRECTION('axis',(0.,0.,1.));
#11949=DIRECTION('refdir',(1.,0.,0.));
#11950=DIRECTION('center_axis',(0.,0.,1.));
#11951=DIRECTION('ref_axis',(1.,0.,0.));
#11952=DIRECTION('center_axis',(0.,0.,-1.));
#11953=DIRECTION('ref_axis',(1.,0.,0.));
#11954=DIRECTION('',(0.,0.,-1.));
#11955=DIRECTION('center_axis',(0.,0.,-1.));
#11956=DIRECTION('ref_axis',(1.,0.,0.));
#11957=DIRECTION('center_axis',(0.,0.,1.));
#11958=DIRECTION('ref_axis',(1.,0.,0.));
#11959=DIRECTION('center_axis',(0.,0.,1.));
#11960=DIRECTION('ref_axis',(1.,0.,0.));
#11961=DIRECTION('',(0.,0.,-1.));
#11962=DIRECTION('center_axis',(0.,0.,1.));
#11963=DIRECTION('ref_axis',(1.,0.,0.));
#11964=DIRECTION('center_axis',(0.,0.,1.));
#11965=DIRECTION('ref_axis',(1.,0.,0.));
#11966=DIRECTION('center_axis',(0.,0.,1.));
#11967=DIRECTION('ref_axis',(1.,0.,0.));
#11968=DIRECTION('axis',(0.,0.,1.));
#11969=DIRECTION('refdir',(1.,0.,0.));
#11970=DIRECTION('center_axis',(-0.000133356257939316,0.990604928518337,
0.136754735973894));
#11971=DIRECTION('ref_axis',(1.84100635426204E-5,-0.136754734734703,0.990604937494615));
#11972=DIRECTION('center_axis',(0.000133356514931307,0.990604928490669,
0.136754736174063));
#11973=DIRECTION('ref_axis',(-0.722226697922822,0.0946826992832939,-0.68514508190888));
#11974=DIRECTION('center_axis',(0.000133356514931307,0.990604928490669,
0.136754736174063));
#11975=DIRECTION('ref_axis',(-0.722226697922822,0.0946826992832939,-0.68514508190888));
#11976=DIRECTION('center_axis',(-0.000133356257939316,0.990604928518337,
0.136754735973894));
#11977=DIRECTION('ref_axis',(1.84100635426204E-5,-0.136754734734703,0.990604937494615));
#11978=DIRECTION('axis',(0.,0.,1.));
#11979=DIRECTION('refdir',(1.,0.,0.));
#11980=DIRECTION('center_axis',(0.,0.,1.));
#11981=DIRECTION('ref_axis',(1.,0.,0.));
#11982=DIRECTION('center_axis',(0.,0.,1.));
#11983=DIRECTION('ref_axis',(1.,0.,0.));
#11984=DIRECTION('',(0.,0.,1.));
#11985=DIRECTION('center_axis',(0.,0.,1.));
#11986=DIRECTION('ref_axis',(1.,0.,0.));
#11987=DIRECTION('center_axis',(0.,0.,1.));
#11988=DIRECTION('ref_axis',(1.,0.,0.));
#11989=DIRECTION('center_axis',(0.,0.,1.));
#11990=DIRECTION('ref_axis',(1.,0.,0.));
#11991=DIRECTION('center_axis',(0.,0.,1.));
#11992=DIRECTION('ref_axis',(1.,0.,0.));
#11993=DIRECTION('',(0.,0.,1.));
#11994=DIRECTION('center_axis',(0.,0.,1.));
#11995=DIRECTION('ref_axis',(1.,0.,0.));
#11996=DIRECTION('center_axis',(0.,0.,1.));
#11997=DIRECTION('ref_axis',(1.,0.,0.));
#11998=DIRECTION('center_axis',(0.,1.,0.));
#11999=DIRECTION('ref_axis',(1.,0.,0.));
#12000=DIRECTION('center_axis',(0.,1.,0.));
#12001=DIRECTION('ref_axis',(1.,0.,0.));
#12002=DIRECTION('',(0.,1.,0.));
#12003=DIRECTION('center_axis',(0.,-1.,0.));
#12004=DIRECTION('ref_axis',(1.,0.,0.));
#12005=DIRECTION('center_axis',(0.,1.,0.));
#12006=DIRECTION('ref_axis',(1.,0.,0.));
#12007=DIRECTION('center_axis',(0.,1.,0.));
#12008=DIRECTION('ref_axis',(1.,0.,0.));
#12009=DIRECTION('',(0.,1.,0.));
#12010=DIRECTION('center_axis',(0.,-1.,0.));
#12011=DIRECTION('ref_axis',(1.,0.,0.));
#12012=DIRECTION('center_axis',(0.,1.,0.));
#12013=DIRECTION('ref_axis',(-1.,0.,0.));
#12014=DIRECTION('',(-1.,0.,0.));
#12015=DIRECTION('',(0.,0.,1.));
#12016=DIRECTION('',(-1.,0.,0.));
#12017=DIRECTION('',(0.,0.,1.));
#12018=DIRECTION('center_axis',(1.,0.,0.));
#12019=DIRECTION('ref_axis',(0.,1.,0.));
#12020=DIRECTION('',(0.,1.,0.));
#12021=DIRECTION('',(0.,1.,0.));
#12022=DIRECTION('',(0.,0.,1.));
#12023=DIRECTION('center_axis',(0.,-1.,0.));
#12024=DIRECTION('ref_axis',(1.,0.,0.));
#12025=DIRECTION('',(1.,0.,0.));
#12026=DIRECTION('',(1.,0.,0.));
#12027=DIRECTION('',(0.,0.,1.));
#12028=DIRECTION('center_axis',(-1.,0.,0.));
#12029=DIRECTION('ref_axis',(0.,-1.,0.));
#12030=DIRECTION('',(0.,-1.,0.));
#12031=DIRECTION('',(0.,-1.,0.));
#12032=DIRECTION('center_axis',(0.,0.,1.));
#12033=DIRECTION('ref_axis',(1.,0.,0.));
#12034=DIRECTION('center_axis',(0.,0.,1.));
#12035=DIRECTION('ref_axis',(1.,0.,0.));
#12036=DIRECTION('axis',(0.,0.,1.));
#12037=DIRECTION('refdir',(1.,0.,0.));
#12038=DIRECTION('center_axis',(0.,0.,1.));
#12039=DIRECTION('ref_axis',(1.,0.,0.));
#12040=DIRECTION('center_axis',(0.,0.,1.));
#12041=DIRECTION('ref_axis',(1.,0.,0.));
#12042=DIRECTION('',(0.,0.,1.));
#12043=DIRECTION('center_axis',(0.,0.,-1.));
#12044=DIRECTION('ref_axis',(1.,0.,0.));
#12045=DIRECTION('center_axis',(0.,0.,1.));
#12046=DIRECTION('ref_axis',(1.,0.,0.));
#12047=DIRECTION('center_axis',(0.,0.,1.));
#12048=DIRECTION('ref_axis',(1.,0.,0.));
#12049=DIRECTION('',(0.,0.,1.));
#12050=DIRECTION('center_axis',(0.,0.,-1.));
#12051=DIRECTION('ref_axis',(1.,0.,0.));
#12052=DIRECTION('center_axis',(0.,1.,0.));
#12053=DIRECTION('ref_axis',(1.,0.,0.));
#12054=DIRECTION('center_axis',(0.,1.,0.));
#12055=DIRECTION('ref_axis',(1.,0.,0.));
#12056=DIRECTION('',(0.,1.,0.));
#12057=DIRECTION('center_axis',(0.,1.,0.));
#12058=DIRECTION('ref_axis',(1.,0.,0.));
#12059=DIRECTION('',(0.,1.,0.));
#12060=DIRECTION('center_axis',(0.,-1.,0.));
#12061=DIRECTION('ref_axis',(1.,0.,0.));
#12062=DIRECTION('',(0.,-1.,0.));
#12063=DIRECTION('center_axis',(0.,1.,0.));
#12064=DIRECTION('ref_axis',(1.,0.,0.));
#12065=DIRECTION('center_axis',(0.,1.,0.));
#12066=DIRECTION('ref_axis',(1.,0.,0.));
#12067=DIRECTION('',(-1.,0.,0.));
#12068=DIRECTION('center_axis',(0.,1.,0.));
#12069=DIRECTION('ref_axis',(1.,0.,0.));
#12070=DIRECTION('center_axis',(0.,1.,0.));
#12071=DIRECTION('ref_axis',(1.,0.,0.));
#12072=DIRECTION('',(0.,1.,0.));
#12073=DIRECTION('center_axis',(0.,1.,0.));
#12074=DIRECTION('ref_axis',(1.,0.,0.));
#12075=DIRECTION('',(0.,1.,0.));
#12076=DIRECTION('center_axis',(0.,-1.,0.));
#12077=DIRECTION('ref_axis',(1.,0.,0.));
#12078=DIRECTION('',(0.,-1.,0.));
#12079=DIRECTION('center_axis',(0.,1.,0.));
#12080=DIRECTION('ref_axis',(1.,0.,0.));
#12081=DIRECTION('center_axis',(0.,1.,0.));
#12082=DIRECTION('ref_axis',(1.,0.,0.));
#12083=DIRECTION('',(-1.,0.,0.));
#12084=DIRECTION('center_axis',(0.,1.,0.));
#12085=DIRECTION('ref_axis',(-1.,0.,0.));
#12086=DIRECTION('',(1.,0.,0.));
#12087=DIRECTION('',(1.,0.,0.));
#12088=DIRECTION('',(0.,0.,1.));
#12089=DIRECTION('',(-1.,0.,0.));
#12090=DIRECTION('',(0.,0.,1.));
#12091=DIRECTION('',(1.,0.,0.));
#12092=DIRECTION('center_axis',(0.,0.,-1.));
#12093=DIRECTION('ref_axis',(-1.,0.,0.));
#12094=DIRECTION('',(0.,1.,0.));
#12095=DIRECTION('',(-1.,0.,0.));
#12096=DIRECTION('',(0.,1.,0.));
#12097=DIRECTION('center_axis',(0.,1.,0.));
#12098=DIRECTION('ref_axis',(0.,0.,1.));
#12099=DIRECTION('',(1.,0.,0.));
#12100=DIRECTION('',(0.,0.,-1.));
#12101=DIRECTION('',(0.,0.,1.));
#12102=DIRECTION('center_axis',(1.,0.,0.));
#12103=DIRECTION('ref_axis',(0.,1.,0.));
#12104=DIRECTION('',(0.,0.,1.));
#12105=DIRECTION('',(0.,1.,0.));
#12106=DIRECTION('',(0.,1.,0.));
#12107=DIRECTION('center_axis',(0.,-1.,0.));
#12108=DIRECTION('ref_axis',(1.,0.,0.));
#12109=DIRECTION('',(0.,0.,1.));
#12110=DIRECTION('',(1.,0.,0.));
#12111=DIRECTION('',(1.,0.,0.));
#12112=DIRECTION('center_axis',(-1.,0.,0.));
#12113=DIRECTION('ref_axis',(0.,-1.,0.));
#12114=DIRECTION('',(0.,-1.,0.));
#12115=DIRECTION('',(0.,1.,0.));
#12116=DIRECTION('center_axis',(0.,0.,1.));
#12117=DIRECTION('ref_axis',(1.,0.,0.));
#12118=DIRECTION('center_axis',(0.,0.,1.));
#12119=DIRECTION('ref_axis',(1.,0.,0.));
#12120=DIRECTION('axis',(0.,0.,1.));
#12121=DIRECTION('refdir',(1.,0.,0.));
#12122=DIRECTION('center_axis',(0.,0.,1.));
#12123=DIRECTION('ref_axis',(1.,0.,0.));
#12124=DIRECTION('center_axis',(0.,0.,-1.));
#12125=DIRECTION('ref_axis',(1.,0.,0.));
#12126=DIRECTION('',(0.,0.,-1.));
#12127=DIRECTION('center_axis',(0.,0.,-1.));
#12128=DIRECTION('ref_axis',(1.,0.,0.));
#12129=DIRECTION('center_axis',(0.,0.,1.));
#12130=DIRECTION('ref_axis',(1.,0.,0.));
#12131=DIRECTION('center_axis',(0.,0.,1.));
#12132=DIRECTION('ref_axis',(1.,0.,0.));
#12133=DIRECTION('',(0.,0.,-1.));
#12134=DIRECTION('center_axis',(0.,0.,1.));
#12135=DIRECTION('ref_axis',(1.,0.,0.));
#12136=DIRECTION('center_axis',(0.,0.,1.));
#12137=DIRECTION('ref_axis',(1.,0.,0.));
#12138=DIRECTION('center_axis',(0.,0.,1.));
#12139=DIRECTION('ref_axis',(1.,0.,0.));
#12140=DIRECTION('axis',(0.,0.,1.));
#12141=DIRECTION('refdir',(1.,0.,0.));
#12142=DIRECTION('center_axis',(-0.000133356251592195,0.990604928516511,
0.136754735987128));
#12143=DIRECTION('ref_axis',(1.84100626682885E-5,-0.136754734747938,0.990604937492788));
#12144=DIRECTION('center_axis',(0.000133356514576091,0.990604928496106,
0.136754736134679));
#12145=DIRECTION('ref_axis',(-0.72222669792222,0.0946826992558859,-0.685145081913302));
#12146=DIRECTION('center_axis',(0.000133356514576091,0.990604928496106,
0.136754736134679));
#12147=DIRECTION('ref_axis',(-0.72222669792222,0.0946826992558859,-0.685145081913302));
#12148=DIRECTION('center_axis',(-0.000133356251592195,0.990604928516511,
0.136754735987128));
#12149=DIRECTION('ref_axis',(1.84100626682885E-5,-0.136754734747938,0.990604937492788));
#12150=DIRECTION('axis',(0.,0.,1.));
#12151=DIRECTION('refdir',(1.,0.,0.));
#12152=DIRECTION('center_axis',(0.,0.,1.));
#12153=DIRECTION('ref_axis',(1.,0.,0.));
#12154=DIRECTION('center_axis',(0.,0.,1.));
#12155=DIRECTION('ref_axis',(1.,0.,0.));
#12156=DIRECTION('',(0.,0.,1.));
#12157=DIRECTION('center_axis',(0.,0.,1.));
#12158=DIRECTION('ref_axis',(1.,0.,0.));
#12159=DIRECTION('center_axis',(0.,0.,1.));
#12160=DIRECTION('ref_axis',(1.,0.,0.));
#12161=DIRECTION('center_axis',(0.,0.,1.));
#12162=DIRECTION('ref_axis',(1.,0.,0.));
#12163=DIRECTION('center_axis',(0.,0.,1.));
#12164=DIRECTION('ref_axis',(1.,0.,0.));
#12165=DIRECTION('',(0.,0.,1.));
#12166=DIRECTION('center_axis',(0.,0.,1.));
#12167=DIRECTION('ref_axis',(1.,0.,0.));
#12168=DIRECTION('center_axis',(0.,0.,1.));
#12169=DIRECTION('ref_axis',(1.,0.,0.));
#12170=DIRECTION('center_axis',(0.,0.,1.));
#12171=DIRECTION('ref_axis',(1.,0.,0.));
#12172=DIRECTION('center_axis',(0.,0.,1.));
#12173=DIRECTION('ref_axis',(1.,0.,0.));
#12174=DIRECTION('',(0.,0.,1.));
#12175=DIRECTION('center_axis',(0.,0.,1.));
#12176=DIRECTION('ref_axis',(1.,0.,0.));
#12177=DIRECTION('center_axis',(0.,0.,1.));
#12178=DIRECTION('ref_axis',(1.,0.,0.));
#12179=DIRECTION('center_axis',(0.,0.,1.));
#12180=DIRECTION('ref_axis',(1.,0.,0.));
#12181=DIRECTION('center_axis',(0.,0.,1.));
#12182=DIRECTION('ref_axis',(1.,0.,0.));
#12183=DIRECTION('',(0.,0.,1.));
#12184=DIRECTION('center_axis',(0.,0.,1.));
#12185=DIRECTION('ref_axis',(1.,0.,0.));
#12186=DIRECTION('center_axis',(0.,0.,1.));
#12187=DIRECTION('ref_axis',(1.,0.,0.));
#12188=DIRECTION('center_axis',(0.,0.,1.));
#12189=DIRECTION('ref_axis',(1.,0.,0.));
#12190=DIRECTION('center_axis',(0.,0.,1.));
#12191=DIRECTION('ref_axis',(1.,0.,0.));
#12192=DIRECTION('',(0.,0.,1.));
#12193=DIRECTION('center_axis',(0.,0.,-1.));
#12194=DIRECTION('ref_axis',(1.,0.,0.));
#12195=DIRECTION('center_axis',(0.,0.,1.));
#12196=DIRECTION('ref_axis',(1.,0.,0.));
#12197=DIRECTION('center_axis',(0.,0.,1.));
#12198=DIRECTION('ref_axis',(1.,0.,0.));
#12199=DIRECTION('center_axis',(0.,0.,1.));
#12200=DIRECTION('ref_axis',(1.,0.,0.));
#12201=DIRECTION('',(0.,0.,1.));
#12202=DIRECTION('center_axis',(0.,0.,-1.));
#12203=DIRECTION('ref_axis',(1.,0.,0.));
#12204=DIRECTION('center_axis',(0.,0.,1.));
#12205=DIRECTION('ref_axis',(1.,0.,0.));
#12206=DIRECTION('center_axis',(0.,1.,0.));
#12207=DIRECTION('ref_axis',(-1.,0.,0.));
#12208=DIRECTION('',(-1.,0.,0.));
#12209=DIRECTION('',(0.,0.,1.));
#12210=DIRECTION('',(-1.,0.,0.));
#12211=DIRECTION('',(0.,0.,1.));
#12212=DIRECTION('center_axis',(1.,0.,0.));
#12213=DIRECTION('ref_axis',(0.,1.,0.));
#12214=DIRECTION('',(0.,1.,0.));
#12215=DIRECTION('',(0.,1.,0.));
#12216=DIRECTION('',(0.,0.,1.));
#12217=DIRECTION('center_axis',(0.,-1.,0.));
#12218=DIRECTION('ref_axis',(1.,0.,0.));
#12219=DIRECTION('',(1.,0.,0.));
#12220=DIRECTION('',(1.,0.,0.));
#12221=DIRECTION('',(0.,0.,1.));
#12222=DIRECTION('center_axis',(-1.,0.,0.));
#12223=DIRECTION('ref_axis',(0.,-1.,0.));
#12224=DIRECTION('',(0.,-1.,0.));
#12225=DIRECTION('',(0.,-1.,0.));
#12226=DIRECTION('center_axis',(0.,0.,1.));
#12227=DIRECTION('ref_axis',(1.,0.,0.));
#12228=DIRECTION('center_axis',(0.,0.,1.));
#12229=DIRECTION('ref_axis',(1.,0.,0.));
#12230=DIRECTION('axis',(0.,0.,1.));
#12231=DIRECTION('refdir',(1.,0.,0.));
#12232=DIRECTION('center_axis',(0.,0.,1.));
#12233=DIRECTION('ref_axis',(1.,0.,0.));
#12234=DIRECTION('center_axis',(0.,0.,1.));
#12235=DIRECTION('ref_axis',(1.,0.,0.));
#12236=DIRECTION('',(0.,0.,1.));
#12237=DIRECTION('center_axis',(0.,0.,-1.));
#12238=DIRECTION('ref_axis',(1.,0.,0.));
#12239=DIRECTION('center_axis',(0.,0.,1.));
#12240=DIRECTION('ref_axis',(1.,0.,0.));
#12241=DIRECTION('center_axis',(0.,0.,1.));
#12242=DIRECTION('ref_axis',(1.,0.,0.));
#12243=DIRECTION('',(0.,0.,1.));
#12244=DIRECTION('center_axis',(0.,0.,-1.));
#12245=DIRECTION('ref_axis',(1.,0.,0.));
#12246=DIRECTION('center_axis',(0.,0.,1.));
#12247=DIRECTION('ref_axis',(1.,0.,0.));
#12248=DIRECTION('center_axis',(0.,0.,1.));
#12249=DIRECTION('ref_axis',(1.,0.,0.));
#12250=DIRECTION('',(0.,0.,1.));
#12251=DIRECTION('center_axis',(0.,0.,-1.));
#12252=DIRECTION('ref_axis',(1.,0.,0.));
#12253=DIRECTION('center_axis',(0.,0.,1.));
#12254=DIRECTION('ref_axis',(1.,0.,0.));
#12255=DIRECTION('center_axis',(0.,0.,1.));
#12256=DIRECTION('ref_axis',(1.,0.,0.));
#12257=DIRECTION('',(0.,0.,1.));
#12258=DIRECTION('center_axis',(0.,0.,-1.));
#12259=DIRECTION('ref_axis',(1.,0.,0.));
#12260=DIRECTION('center_axis',(0.,0.,1.));
#12261=DIRECTION('ref_axis',(1.,0.,0.));
#12262=DIRECTION('center_axis',(0.,0.,1.));
#12263=DIRECTION('ref_axis',(1.,0.,0.));
#12264=DIRECTION('',(0.,0.,1.));
#12265=DIRECTION('center_axis',(0.,0.,-1.));
#12266=DIRECTION('ref_axis',(1.,0.,0.));
#12267=DIRECTION('center_axis',(0.,0.,1.));
#12268=DIRECTION('ref_axis',(1.,0.,0.));
#12269=DIRECTION('center_axis',(0.,0.,1.));
#12270=DIRECTION('ref_axis',(1.,0.,0.));
#12271=DIRECTION('',(0.,0.,1.));
#12272=DIRECTION('center_axis',(0.,0.,-1.));
#12273=DIRECTION('ref_axis',(1.,0.,0.));
#12274=DIRECTION('center_axis',(0.,0.,1.));
#12275=DIRECTION('ref_axis',(1.,0.,0.));
#12276=DIRECTION('center_axis',(0.,0.,1.));
#12277=DIRECTION('ref_axis',(1.,0.,0.));
#12278=DIRECTION('',(0.,0.,1.));
#12279=DIRECTION('center_axis',(0.,0.,-1.));
#12280=DIRECTION('ref_axis',(1.,0.,0.));
#12281=DIRECTION('center_axis',(0.,0.,1.));
#12282=DIRECTION('ref_axis',(1.,0.,0.));
#12283=DIRECTION('center_axis',(0.,0.,1.));
#12284=DIRECTION('ref_axis',(1.,0.,0.));
#12285=DIRECTION('',(0.,0.,1.));
#12286=DIRECTION('center_axis',(0.,0.,-1.));
#12287=DIRECTION('ref_axis',(1.,0.,0.));
#12288=DIRECTION('center_axis',(0.,1.,0.));
#12289=DIRECTION('ref_axis',(-1.,0.,0.));
#12290=DIRECTION('',(-1.,0.,0.));
#12291=DIRECTION('',(0.,0.,1.));
#12292=DIRECTION('',(-1.,0.,0.));
#12293=DIRECTION('',(0.,0.,1.));
#12294=DIRECTION('center_axis',(1.,0.,0.));
#12295=DIRECTION('ref_axis',(0.,1.,0.));
#12296=DIRECTION('',(0.,1.,0.));
#12297=DIRECTION('',(0.,1.,0.));
#12298=DIRECTION('',(0.,0.,1.));
#12299=DIRECTION('center_axis',(0.,-1.,0.));
#12300=DIRECTION('ref_axis',(1.,0.,0.));
#12301=DIRECTION('',(1.,0.,0.));
#12302=DIRECTION('',(1.,0.,0.));
#12303=DIRECTION('',(0.,0.,1.));
#12304=DIRECTION('center_axis',(-1.,0.,0.));
#12305=DIRECTION('ref_axis',(0.,-1.,0.));
#12306=DIRECTION('',(0.,-1.,0.));
#12307=DIRECTION('',(0.,-1.,0.));
#12308=DIRECTION('center_axis',(0.,0.,1.));
#12309=DIRECTION('ref_axis',(1.,0.,0.));
#12310=DIRECTION('center_axis',(0.,0.,1.));
#12311=DIRECTION('ref_axis',(1.,0.,0.));
#12312=DIRECTION('axis',(0.,0.,1.));
#12313=DIRECTION('refdir',(1.,0.,0.));
#12314=DIRECTION('center_axis',(0.,0.,1.));
#12315=DIRECTION('ref_axis',(1.,0.,0.));
#12316=DIRECTION('center_axis',(0.,0.,-1.));
#12317=DIRECTION('ref_axis',(1.,0.,0.));
#12318=DIRECTION('',(0.,0.,-1.));
#12319=DIRECTION('center_axis',(0.,0.,-1.));
#12320=DIRECTION('ref_axis',(1.,0.,0.));
#12321=DIRECTION('center_axis',(0.,0.,1.));
#12322=DIRECTION('ref_axis',(1.,0.,0.));
#12323=DIRECTION('center_axis',(0.,0.,1.));
#12324=DIRECTION('ref_axis',(1.,0.,0.));
#12325=DIRECTION('',(0.,0.,-1.));
#12326=DIRECTION('center_axis',(0.,0.,1.));
#12327=DIRECTION('ref_axis',(1.,0.,0.));
#12328=DIRECTION('center_axis',(0.,0.,1.));
#12329=DIRECTION('ref_axis',(1.,0.,0.));
#12330=DIRECTION('center_axis',(0.,0.,1.));
#12331=DIRECTION('ref_axis',(1.,0.,0.));
#12332=DIRECTION('axis',(0.,0.,1.));
#12333=DIRECTION('refdir',(1.,0.,0.));
#12334=DIRECTION('center_axis',(0.,0.,1.));
#12335=DIRECTION('ref_axis',(1.,0.,0.));
#12336=DIRECTION('center_axis',(0.,0.,1.));
#12337=DIRECTION('ref_axis',(1.,0.,0.));
#12338=DIRECTION('',(0.,0.,1.));
#12339=DIRECTION('center_axis',(0.,0.,1.));
#12340=DIRECTION('ref_axis',(1.,0.,0.));
#12341=DIRECTION('center_axis',(0.,0.,1.));
#12342=DIRECTION('ref_axis',(1.,0.,0.));
#12343=DIRECTION('center_axis',(0.,0.,1.));
#12344=DIRECTION('ref_axis',(1.,0.,0.));
#12345=DIRECTION('center_axis',(0.,0.,1.));
#12346=DIRECTION('ref_axis',(1.,0.,0.));
#12347=DIRECTION('',(0.,0.,-1.));
#12348=DIRECTION('center_axis',(0.,0.,1.));
#12349=DIRECTION('ref_axis',(1.,0.,0.));
#12350=DIRECTION('center_axis',(0.,0.,1.));
#12351=DIRECTION('ref_axis',(1.,0.,0.));
#12352=DIRECTION('center_axis',(0.,0.,1.));
#12353=DIRECTION('ref_axis',(1.,0.,0.));
#12354=DIRECTION('axis',(0.,0.,1.));
#12355=DIRECTION('refdir',(1.,0.,0.));
#12356=DIRECTION('center_axis',(0.,0.,1.));
#12357=DIRECTION('ref_axis',(1.,0.,0.));
#12358=DIRECTION('center_axis',(0.,0.,1.));
#12359=DIRECTION('ref_axis',(1.,0.,0.));
#12360=DIRECTION('',(0.,0.,-1.));
#12361=DIRECTION('center_axis',(0.,0.,1.));
#12362=DIRECTION('ref_axis',(1.,0.,0.));
#12363=DIRECTION('center_axis',(0.,0.,1.));
#12364=DIRECTION('ref_axis',(1.,0.,0.));
#12365=DIRECTION('center_axis',(0.,0.,1.));
#12366=DIRECTION('ref_axis',(1.,0.,0.));
#12367=DIRECTION('axis',(0.,0.,1.));
#12368=DIRECTION('refdir',(1.,0.,0.));
#12369=DIRECTION('center_axis',(0.,0.,1.));
#12370=DIRECTION('ref_axis',(1.,0.,0.));
#12371=DIRECTION('center_axis',(0.,0.,1.));
#12372=DIRECTION('ref_axis',(1.,0.,0.));
#12373=DIRECTION('',(0.,0.,1.));
#12374=DIRECTION('center_axis',(0.,0.,-1.));
#12375=DIRECTION('ref_axis',(1.,0.,0.));
#12376=DIRECTION('center_axis',(0.,0.,1.));
#12377=DIRECTION('ref_axis',(1.,0.,0.));
#12378=DIRECTION('center_axis',(0.,0.,1.));
#12379=DIRECTION('ref_axis',(1.,0.,0.));
#12380=DIRECTION('center_axis',(0.,0.,1.));
#12381=DIRECTION('ref_axis',(1.,0.,0.));
#12382=DIRECTION('',(0.,0.,-1.));
#12383=DIRECTION('center_axis',(0.,0.,1.));
#12384=DIRECTION('ref_axis',(1.,0.,0.));
#12385=DIRECTION('center_axis',(0.,0.,1.));
#12386=DIRECTION('ref_axis',(1.,0.,0.));
#12387=DIRECTION('center_axis',(0.,0.,1.));
#12388=DIRECTION('ref_axis',(1.,0.,0.));
#12389=DIRECTION('axis',(0.,0.,1.));
#12390=DIRECTION('refdir',(1.,0.,0.));
#12391=DIRECTION('center_axis',(0.,0.,1.));
#12392=DIRECTION('ref_axis',(1.,0.,0.));
#12393=DIRECTION('center_axis',(0.,0.,1.));
#12394=DIRECTION('ref_axis',(1.,0.,0.));
#12395=DIRECTION('',(0.,0.,-1.));
#12396=DIRECTION('center_axis',(0.,0.,1.));
#12397=DIRECTION('ref_axis',(1.,0.,0.));
#12398=DIRECTION('center_axis',(0.,0.,1.));
#12399=DIRECTION('ref_axis',(1.,0.,0.));
#12400=DIRECTION('center_axis',(0.,0.,1.));
#12401=DIRECTION('ref_axis',(1.,0.,0.));
#12402=DIRECTION('axis',(0.,0.,1.));
#12403=DIRECTION('refdir',(1.,0.,0.));
#12404=DIRECTION('center_axis',(0.,0.,1.));
#12405=DIRECTION('ref_axis',(1.,0.,0.));
#12406=DIRECTION('center_axis',(0.,0.,1.));
#12407=DIRECTION('ref_axis',(1.,0.,0.));
#12408=DIRECTION('',(0.,0.,1.));
#12409=DIRECTION('center_axis',(0.,0.,1.));
#12410=DIRECTION('ref_axis',(1.,0.,0.));
#12411=DIRECTION('center_axis',(0.,0.,1.));
#12412=DIRECTION('ref_axis',(1.,0.,0.));
#12413=DIRECTION('center_axis',(0.,0.,1.));
#12414=DIRECTION('ref_axis',(1.,0.,0.));
#12415=DIRECTION('center_axis',(0.,0.,1.));
#12416=DIRECTION('ref_axis',(1.,0.,0.));
#12417=DIRECTION('',(0.,0.,-1.));
#12418=DIRECTION('center_axis',(0.,0.,1.));
#12419=DIRECTION('ref_axis',(1.,0.,0.));
#12420=DIRECTION('center_axis',(0.,0.,1.));
#12421=DIRECTION('ref_axis',(1.,0.,0.));
#12422=DIRECTION('center_axis',(0.,0.,1.));
#12423=DIRECTION('ref_axis',(1.,0.,0.));
#12424=DIRECTION('axis',(0.,0.,1.));
#12425=DIRECTION('refdir',(1.,0.,0.));
#12426=DIRECTION('center_axis',(0.,0.,1.));
#12427=DIRECTION('ref_axis',(1.,0.,0.));
#12428=DIRECTION('center_axis',(0.,0.,1.));
#12429=DIRECTION('ref_axis',(1.,0.,0.));
#12430=DIRECTION('',(0.,0.,-1.));
#12431=DIRECTION('center_axis',(0.,0.,1.));
#12432=DIRECTION('ref_axis',(1.,0.,0.));
#12433=DIRECTION('center_axis',(0.,0.,1.));
#12434=DIRECTION('ref_axis',(1.,0.,0.));
#12435=DIRECTION('center_axis',(0.,0.,1.));
#12436=DIRECTION('ref_axis',(1.,0.,0.));
#12437=DIRECTION('axis',(0.,0.,1.));
#12438=DIRECTION('refdir',(1.,0.,0.));
#12439=DIRECTION('center_axis',(0.,0.,1.));
#12440=DIRECTION('ref_axis',(1.,0.,0.));
#12441=DIRECTION('center_axis',(0.,0.,1.));
#12442=DIRECTION('ref_axis',(1.,0.,0.));
#12443=DIRECTION('',(0.,0.,1.));
#12444=DIRECTION('center_axis',(0.,0.,-1.));
#12445=DIRECTION('ref_axis',(1.,0.,0.));
#12446=DIRECTION('center_axis',(0.,0.,1.));
#12447=DIRECTION('ref_axis',(1.,0.,0.));
#12448=DIRECTION('center_axis',(0.,0.,1.));
#12449=DIRECTION('ref_axis',(1.,0.,0.));
#12450=DIRECTION('center_axis',(0.,0.,1.));
#12451=DIRECTION('ref_axis',(1.,0.,0.));
#12452=DIRECTION('',(0.,0.,-1.));
#12453=DIRECTION('center_axis',(0.,0.,1.));
#12454=DIRECTION('ref_axis',(1.,0.,0.));
#12455=DIRECTION('center_axis',(0.,0.,1.));
#12456=DIRECTION('ref_axis',(1.,0.,0.));
#12457=DIRECTION('center_axis',(0.,0.,1.));
#12458=DIRECTION('ref_axis',(1.,0.,0.));
#12459=DIRECTION('axis',(0.,0.,1.));
#12460=DIRECTION('refdir',(1.,0.,0.));
#12461=DIRECTION('center_axis',(0.,0.,1.));
#12462=DIRECTION('ref_axis',(1.,0.,0.));
#12463=DIRECTION('center_axis',(0.,0.,1.));
#12464=DIRECTION('ref_axis',(1.,0.,0.));
#12465=DIRECTION('',(0.,0.,-1.));
#12466=DIRECTION('center_axis',(0.,0.,1.));
#12467=DIRECTION('ref_axis',(1.,0.,0.));
#12468=DIRECTION('center_axis',(0.,0.,1.));
#12469=DIRECTION('ref_axis',(1.,0.,0.));
#12470=DIRECTION('center_axis',(0.,0.,1.));
#12471=DIRECTION('ref_axis',(1.,0.,0.));
#12472=DIRECTION('axis',(0.,0.,1.));
#12473=DIRECTION('refdir',(1.,0.,0.));
#12474=DIRECTION('center_axis',(1.,0.,0.));
#12475=DIRECTION('ref_axis',(0.,0.,-1.));
#12476=DIRECTION('center_axis',(-1.,0.,0.));
#12477=DIRECTION('ref_axis',(0.,0.,-1.));
#12478=DIRECTION('',(-0.707106781186548,8.65956056235493E-17,-0.707106781186547));
#12479=DIRECTION('center_axis',(1.,0.,0.));
#12480=DIRECTION('ref_axis',(0.,0.,-1.));
#12481=DIRECTION('center_axis',(1.,0.,0.));
#12482=DIRECTION('ref_axis',(0.,0.,-1.));
#12483=DIRECTION('center_axis',(1.,0.,0.));
#12484=DIRECTION('ref_axis',(0.,0.,-1.));
#12485=DIRECTION('',(-1.,0.,0.));
#12486=DIRECTION('center_axis',(1.,0.,0.));
#12487=DIRECTION('ref_axis',(0.,0.,-1.));
#12488=DIRECTION('center_axis',(-1.,0.,0.));
#12489=DIRECTION('ref_axis',(0.,0.,-1.));
#12490=DIRECTION('center_axis',(-1.,0.,0.));
#12491=DIRECTION('ref_axis',(0.,0.,-1.));
#12492=DIRECTION('',(-0.707106781186553,-8.65956056235487E-17,0.707106781186542));
#12493=DIRECTION('center_axis',(1.,0.,0.));
#12494=DIRECTION('ref_axis',(0.,0.,-1.));
#12495=DIRECTION('axis',(0.,0.,1.));
#12496=DIRECTION('refdir',(1.,0.,0.));
#12497=DIRECTION('center_axis',(0.,0.,1.));
#12498=DIRECTION('ref_axis',(1.,0.,0.));
#12499=DIRECTION('',(0.,-1.,0.));
#12500=DIRECTION('center_axis',(0.,0.,1.));
#12501=DIRECTION('ref_axis',(1.,0.,0.));
#12502=DIRECTION('center_axis',(0.,0.,1.));
#12503=DIRECTION('ref_axis',(1.,0.,0.));
#12504=DIRECTION('',(0.,0.,1.));
#12505=DIRECTION('center_axis',(0.,0.,1.));
#12506=DIRECTION('ref_axis',(1.,0.,0.));
#12507=DIRECTION('',(0.,0.,-1.));
#12508=DIRECTION('center_axis',(0.,0.,1.));
#12509=DIRECTION('ref_axis',(-1.,1.22464679914735E-16,0.));
#12510=DIRECTION('',(0.,0.,-1.));
#12511=DIRECTION('center_axis',(0.,0.,1.));
#12512=DIRECTION('ref_axis',(1.,0.,0.));
#12513=DIRECTION('',(0.,0.,1.));
#12514=DIRECTION('center_axis',(0.,0.,1.));
#12515=DIRECTION('ref_axis',(1.,0.,0.));
#12516=DIRECTION('center_axis',(0.,0.,1.));
#12517=DIRECTION('ref_axis',(1.,0.,0.));
#12518=DIRECTION('',(0.,1.,0.));
#12519=DIRECTION('center_axis',(0.,0.,1.));
#12520=DIRECTION('ref_axis',(1.,0.,0.));
#12521=DIRECTION('',(0.,1.,0.));
#12522=DIRECTION('',(1.,0.,0.));
#12523=DIRECTION('',(0.,-1.,0.));
#12524=DIRECTION('',(-1.,0.,0.));
#12525=DIRECTION('',(0.,1.,0.));
#12526=DIRECTION('center_axis',(0.,0.,-1.));
#12527=DIRECTION('ref_axis',(1.,0.,0.));
#12528=DIRECTION('center_axis',(-1.,0.,0.));
#12529=DIRECTION('ref_axis',(0.,0.,1.));
#12530=DIRECTION('',(0.,0.,-1.));
#12531=DIRECTION('',(0.,1.,0.));
#12532=DIRECTION('',(0.,0.,1.));
#12533=DIRECTION('center_axis',(1.,0.,0.));
#12534=DIRECTION('ref_axis',(0.,0.,-1.));
#12535=DIRECTION('center_axis',(0.,0.,1.));
#12536=DIRECTION('ref_axis',(1.,0.,0.));
#12537=DIRECTION('',(0.,1.,0.));
#12538=DIRECTION('',(1.,0.,0.));
#12539=DIRECTION('',(0.,1.,0.));
#12540=DIRECTION('',(0.,1.,0.));
#12541=DIRECTION('',(-1.,0.,0.));
#12542=DIRECTION('center_axis',(0.,0.,-1.));
#12543=DIRECTION('ref_axis',(1.,0.,0.));
#12544=DIRECTION('center_axis',(1.,0.,0.));
#12545=DIRECTION('ref_axis',(0.,0.,-1.));
#12546=DIRECTION('center_axis',(1.,0.,0.));
#12547=DIRECTION('ref_axis',(0.,0.,-1.));
#12548=DIRECTION('',(1.,0.,0.));
#12549=DIRECTION('center_axis',(-1.,0.,0.));
#12550=DIRECTION('ref_axis',(0.,0.,-1.));
#12551=DIRECTION('center_axis',(1.,0.,0.));
#12552=DIRECTION('ref_axis',(0.,0.,-1.));
#12553=DIRECTION('',(1.,0.,0.));
#12554=DIRECTION('center_axis',(-1.,0.,0.));
#12555=DIRECTION('ref_axis',(0.,0.,-1.));
#12556=DIRECTION('center_axis',(0.,0.,1.));
#12557=DIRECTION('ref_axis',(1.,0.,0.));
#12558=DIRECTION('center_axis',(0.,0.,1.));
#12559=DIRECTION('ref_axis',(1.,0.,0.));
#12560=DIRECTION('',(0.,0.,1.));
#12561=DIRECTION('center_axis',(0.,0.,1.));
#12562=DIRECTION('ref_axis',(1.,0.,0.));
#12563=DIRECTION('center_axis',(0.,0.,1.));
#12564=DIRECTION('ref_axis',(1.,0.,0.));
#12565=DIRECTION('',(0.,0.,1.));
#12566=DIRECTION('center_axis',(0.,1.,0.));
#12567=DIRECTION('ref_axis',(1.,0.,0.));
#12568=DIRECTION('center_axis',(0.,1.,0.));
#12569=DIRECTION('ref_axis',(1.,0.,0.));
#12570=DIRECTION('',(0.,1.,0.));
#12571=DIRECTION('center_axis',(0.,-1.,0.));
#12572=DIRECTION('ref_axis',(1.,0.,0.));
#12573=DIRECTION('center_axis',(0.,-1.,0.));
#12574=DIRECTION('ref_axis',(0.,0.,-1.));
#12575=DIRECTION('',(0.,0.,-1.));
#12576=DIRECTION('',(1.,0.,0.));
#12577=DIRECTION('',(0.,0.,1.));
#12578=DIRECTION('',(0.,0.,1.));
#12579=DIRECTION('',(-1.,0.,0.));
#12580=DIRECTION('',(0.,0.,-1.));
#12581=DIRECTION('',(-1.,0.,0.));
#12582=DIRECTION('',(0.,0.,1.));
#12583=DIRECTION('',(-1.,0.,0.));
#12584=DIRECTION('center_axis',(-1.,0.,0.));
#12585=DIRECTION('ref_axis',(0.,0.,1.));
#12586=DIRECTION('',(0.,0.,1.));
#12587=DIRECTION('',(0.,1.,0.));
#12588=DIRECTION('center_axis',(0.,0.,-1.));
#12589=DIRECTION('ref_axis',(-1.,0.,0.));
#12590=DIRECTION('',(-1.,0.,0.));
#12591=DIRECTION('',(0.,1.,0.));
#12592=DIRECTION('center_axis',(1.,0.,0.));
#12593=DIRECTION('ref_axis',(0.,0.,-1.));
#12594=DIRECTION('',(0.,0.,-1.));
#12595=DIRECTION('center_axis',(1.,0.,0.));
#12596=DIRECTION('ref_axis',(0.,0.,-1.));
#12597=DIRECTION('',(0.,0.,-1.));
#12598=DIRECTION('',(0.,1.,0.));
#12599=DIRECTION('center_axis',(0.,0.,1.));
#12600=DIRECTION('ref_axis',(1.,0.,0.));
#12601=DIRECTION('',(1.,0.,0.));
#12602=DIRECTION('',(0.,1.,0.));
#12603=DIRECTION('center_axis',(-1.,0.,0.));
#12604=DIRECTION('ref_axis',(0.,0.,1.));
#12605=DIRECTION('',(0.,0.,1.));
#12606=DIRECTION('',(0.,1.,0.));
#12607=DIRECTION('center_axis',(0.,0.,1.));
#12608=DIRECTION('ref_axis',(1.,0.,0.));
#12609=DIRECTION('',(1.,0.,0.));
#12610=DIRECTION('',(0.,1.,0.));
#12611=DIRECTION('center_axis',(1.,0.,0.));
#12612=DIRECTION('ref_axis',(0.,0.,-1.));
#12613=DIRECTION('',(0.,0.,-1.));
#12614=DIRECTION('',(0.,1.,0.));
#12615=DIRECTION('center_axis',(0.,0.,1.));
#12616=DIRECTION('ref_axis',(1.,0.,0.));
#12617=DIRECTION('',(1.,0.,0.));
#12618=DIRECTION('center_axis',(0.,1.,0.));
#12619=DIRECTION('ref_axis',(0.,0.,1.));
#12620=DIRECTION('axis',(0.,0.,1.));
#12621=DIRECTION('refdir',(1.,0.,0.));
#12622=DIRECTION('center_axis',(0.866025403784439,0.,-0.5));
#12623=DIRECTION('ref_axis',(0.5,0.,0.866025403784439));
#12624=DIRECTION('',(-0.5,0.,-0.866025403784439));
#12625=DIRECTION('',(0.,-1.,0.));
#12626=DIRECTION('',(0.5,0.,0.866025403784439));
#12627=DIRECTION('',(0.,-1.,0.));
#12628=DIRECTION('center_axis',(1.20185167898973E-16,0.,-1.));
#12629=DIRECTION('ref_axis',(1.,0.,1.20185167898973E-16));
#12630=DIRECTION('',(-1.,0.,-1.20185167898973E-16));
#12631=DIRECTION('',(0.,-1.,0.));
#12632=DIRECTION('',(1.,0.,1.20185167898973E-16));
#12633=DIRECTION('center_axis',(-0.866025403784439,0.,-0.5));
#12634=DIRECTION('ref_axis',(0.5,0.,-0.866025403784439));
#12635=DIRECTION('',(-0.5,0.,0.866025403784439));
#12636=DIRECTION('',(0.,-1.,0.));
#12637=DIRECTION('',(0.5,0.,-0.866025403784439));
#12638=DIRECTION('center_axis',(-0.866025403784439,0.,0.5));
#12639=DIRECTION('ref_axis',(-0.5,0.,-0.866025403784439));
#12640=DIRECTION('',(0.5,0.,0.866025403784439));
#12641=DIRECTION('',(0.,-1.,0.));
#12642=DIRECTION('',(-0.5,0.,-0.866025403784439));
#12643=DIRECTION('center_axis',(-2.40370335797945E-16,0.,1.));
#12644=DIRECTION('ref_axis',(-1.,0.,-2.40370335797945E-16));
#12645=DIRECTION('',(1.,0.,2.40370335797945E-16));
#12646=DIRECTION('',(0.,-1.,0.));
#12647=DIRECTION('',(-1.,0.,-2.40370335797945E-16));
#12648=DIRECTION('center_axis',(0.866025403784439,0.,0.5));
#12649=DIRECTION('ref_axis',(-0.5,0.,0.866025403784439));
#12650=DIRECTION('',(0.5,0.,-0.866025403784439));
#12651=DIRECTION('',(-0.5,0.,0.866025403784439));
#12652=DIRECTION('center_axis',(0.,1.,0.));
#12653=DIRECTION('ref_axis',(1.,0.,0.));
#12654=DIRECTION('center_axis',(0.,-1.,0.));
#12655=DIRECTION('ref_axis',(0.,0.,-1.));
#12656=DIRECTION('center_axis',(0.,1.,0.));
#12657=DIRECTION('ref_axis',(1.,0.,0.));
#12658=DIRECTION('center_axis',(0.,1.,0.));
#12659=DIRECTION('ref_axis',(1.,0.,0.));
#12660=DIRECTION('center_axis',(0.,1.,0.));
#12661=DIRECTION('ref_axis',(0.,0.,1.));
#12662=DIRECTION('center_axis',(0.,-1.,0.));
#12663=DIRECTION('ref_axis',(1.,0.,0.));
#12664=DIRECTION('center_axis',(0.,-1.,0.));
#12665=DIRECTION('ref_axis',(1.,0.,0.));
#12666=DIRECTION('center_axis',(0.,-1.,0.));
#12667=DIRECTION('ref_axis',(1.,0.,0.));
#12668=DIRECTION('',(0.707106781186548,0.707106781186547,8.65956056235493E-17));
#12669=DIRECTION('center_axis',(0.,-1.,0.));
#12670=DIRECTION('ref_axis',(1.,0.,0.));
#12671=DIRECTION('center_axis',(0.,-1.,0.));
#12672=DIRECTION('ref_axis',(1.,0.,0.));
#12673=DIRECTION('',(0.,1.,0.));
#12674=DIRECTION('center_axis',(0.,1.,0.));
#12675=DIRECTION('ref_axis',(1.,0.,0.));
#12676=DIRECTION('center_axis',(0.,-1.,0.));
#12677=DIRECTION('ref_axis',(1.,0.,0.));
#12678=DIRECTION('',(-0.707106781186547,0.707106781186548,-8.65956056235493E-17));
#12679=DIRECTION('center_axis',(0.,-1.,0.));
#12680=DIRECTION('ref_axis',(0.,0.,-1.));
#12681=DIRECTION('center_axis',(0.,-1.,0.));
#12682=DIRECTION('ref_axis',(1.,0.,0.));
#12683=DIRECTION('center_axis',(0.,1.,0.));
#12684=DIRECTION('ref_axis',(1.,0.,0.));
#12685=DIRECTION('center_axis',(0.,1.,0.));
#12686=DIRECTION('ref_axis',(1.,0.,0.));
#12687=DIRECTION('',(-0.447213595499958,0.894427190999916,-5.47678698264203E-17));
#12688=DIRECTION('center_axis',(0.,-1.,0.));
#12689=DIRECTION('ref_axis',(1.,0.,0.));
#12690=DIRECTION('',(0.,1.,0.));
#12691=DIRECTION('axis',(0.,0.,1.));
#12692=DIRECTION('refdir',(1.,0.,0.));
#12693=DIRECTION('center_axis',(0.,1.,0.));
#12694=DIRECTION('ref_axis',(0.,0.,1.));
#12695=DIRECTION('center_axis',(0.,-1.,0.));
#12696=DIRECTION('ref_axis',(1.,0.,0.));
#12697=DIRECTION('center_axis',(0.,-1.,0.));
#12698=DIRECTION('ref_axis',(1.,0.,0.));
#12699=DIRECTION('center_axis',(0.,-1.,0.));
#12700=DIRECTION('ref_axis',(1.,0.,0.));
#12701=DIRECTION('',(0.707106781186548,0.707106781186547,8.65956056235493E-17));
#12702=DIRECTION('center_axis',(0.,-1.,0.));
#12703=DIRECTION('ref_axis',(1.,0.,0.));
#12704=DIRECTION('center_axis',(0.,-1.,0.));
#12705=DIRECTION('ref_axis',(1.,0.,0.));
#12706=DIRECTION('',(0.,1.,0.));
#12707=DIRECTION('center_axis',(0.,1.,0.));
#12708=DIRECTION('ref_axis',(1.,0.,0.));
#12709=DIRECTION('center_axis',(0.,-1.,0.));
#12710=DIRECTION('ref_axis',(1.,0.,0.));
#12711=DIRECTION('',(-0.707106781186547,0.707106781186548,-8.65956056235493E-17));
#12712=DIRECTION('center_axis',(0.,-1.,0.));
#12713=DIRECTION('ref_axis',(0.,0.,-1.));
#12714=DIRECTION('center_axis',(0.,-1.,0.));
#12715=DIRECTION('ref_axis',(1.,0.,0.));
#12716=DIRECTION('center_axis',(0.,1.,0.));
#12717=DIRECTION('ref_axis',(1.,0.,0.));
#12718=DIRECTION('center_axis',(0.,1.,0.));
#12719=DIRECTION('ref_axis',(1.,0.,0.));
#12720=DIRECTION('',(-0.447213595499958,0.894427190999916,-5.47678698264203E-17));
#12721=DIRECTION('center_axis',(0.,-1.,0.));
#12722=DIRECTION('ref_axis',(1.,0.,0.));
#12723=DIRECTION('center_axis',(0.,1.,0.));
#12724=DIRECTION('ref_axis',(1.,0.,0.));
#12725=DIRECTION('',(0.,1.,0.));
#12726=DIRECTION('center_axis',(0.,1.,0.));
#12727=DIRECTION('ref_axis',(1.,0.,0.));
#12728=DIRECTION('center_axis',(0.,-1.,0.));
#12729=DIRECTION('ref_axis',(1.,0.,0.));
#12730=DIRECTION('',(-0.707106781186547,0.707106781186548,-8.65956056235493E-17));
#12731=DIRECTION('center_axis',(0.,-1.,0.));
#12732=DIRECTION('ref_axis',(0.,0.,-1.));
#12733=DIRECTION('center_axis',(0.866025403784439,0.,-0.5));
#12734=DIRECTION('ref_axis',(0.5,0.,0.866025403784439));
#12735=DIRECTION('',(-0.5,0.,-0.866025403784439));
#12736=DIRECTION('',(0.,-1.,0.));
#12737=DIRECTION('',(0.5,0.,0.866025403784439));
#12738=DIRECTION('',(0.,-1.,0.));
#12739=DIRECTION('center_axis',(1.20185167898973E-16,0.,-1.));
#12740=DIRECTION('ref_axis',(1.,0.,1.20185167898973E-16));
#12741=DIRECTION('',(-1.,0.,-1.20185167898973E-16));
#12742=DIRECTION('',(0.,-1.,0.));
#12743=DIRECTION('',(1.,0.,1.20185167898973E-16));
#12744=DIRECTION('center_axis',(-0.866025403784439,0.,-0.5));
#12745=DIRECTION('ref_axis',(0.5,0.,-0.866025403784439));
#12746=DIRECTION('',(-0.5,0.,0.866025403784439));
#12747=DIRECTION('',(0.,-1.,0.));
#12748=DIRECTION('',(0.5,0.,-0.866025403784439));
#12749=DIRECTION('center_axis',(-0.866025403784439,0.,0.5));
#12750=DIRECTION('ref_axis',(-0.5,0.,-0.866025403784439));
#12751=DIRECTION('',(0.5,0.,0.866025403784439));
#12752=DIRECTION('',(0.,-1.,0.));
#12753=DIRECTION('',(-0.5,0.,-0.866025403784439));
#12754=DIRECTION('center_axis',(-2.40370335797945E-16,0.,1.));
#12755=DIRECTION('ref_axis',(-1.,0.,-2.40370335797945E-16));
#12756=DIRECTION('',(1.,0.,2.40370335797945E-16));
#12757=DIRECTION('',(0.,-1.,0.));
#12758=DIRECTION('',(-1.,0.,-2.40370335797945E-16));
#12759=DIRECTION('center_axis',(0.866025403784439,0.,0.5));
#12760=DIRECTION('ref_axis',(-0.5,0.,0.866025403784439));
#12761=DIRECTION('',(0.5,0.,-0.866025403784439));
#12762=DIRECTION('',(-0.5,0.,0.866025403784439));
#12763=DIRECTION('center_axis',(0.,1.,0.));
#12764=DIRECTION('ref_axis',(1.,0.,0.));
#12765=DIRECTION('center_axis',(0.,-1.,0.));
#12766=DIRECTION('ref_axis',(0.,0.,-1.));
#12767=DIRECTION('axis',(0.,0.,1.));
#12768=DIRECTION('refdir',(1.,0.,0.));
#12769=DIRECTION('axis',(0.,0.,1.));
#12770=DIRECTION('refdir',(1.,0.,0.));
#12771=DIRECTION('center_axis',(0.,0.,1.));
#12772=DIRECTION('ref_axis',(1.,0.,0.));
#12773=DIRECTION('center_axis',(0.,0.,1.));
#12774=DIRECTION('ref_axis',(1.,0.,0.));
#12775=DIRECTION('',(0.,0.,1.));
#12776=DIRECTION('center_axis',(0.,0.,-1.));
#12777=DIRECTION('ref_axis',(1.,0.,0.));
#12778=DIRECTION('center_axis',(0.,0.,1.));
#12779=DIRECTION('ref_axis',(1.,0.,0.));
#12780=DIRECTION('center_axis',(0.,0.,1.));
#12781=DIRECTION('ref_axis',(1.,0.,0.));
#12782=DIRECTION('',(0.,0.,1.));
#12783=DIRECTION('center_axis',(0.,0.,-1.));
#12784=DIRECTION('ref_axis',(1.,0.,0.));
#12785=DIRECTION('center_axis',(0.,0.,1.));
#12786=DIRECTION('ref_axis',(1.,0.,0.));
#12787=DIRECTION('center_axis',(0.,0.,1.));
#12788=DIRECTION('ref_axis',(1.,0.,0.));
#12789=DIRECTION('',(0.,0.,1.));
#12790=DIRECTION('center_axis',(0.,0.,-1.));
#12791=DIRECTION('ref_axis',(1.,0.,0.));
#12792=DIRECTION('center_axis',(0.,0.,1.));
#12793=DIRECTION('ref_axis',(1.,0.,0.));
#12794=DIRECTION('center_axis',(0.,0.,1.));
#12795=DIRECTION('ref_axis',(1.,0.,0.));
#12796=DIRECTION('',(0.,0.,1.));
#12797=DIRECTION('center_axis',(0.,0.,-1.));
#12798=DIRECTION('ref_axis',(1.,0.,0.));
#12799=DIRECTION('center_axis',(0.,0.,1.));
#12800=DIRECTION('ref_axis',(1.,0.,0.));
#12801=DIRECTION('center_axis',(0.,0.,1.));
#12802=DIRECTION('ref_axis',(1.,0.,0.));
#12803=DIRECTION('',(0.,0.,1.));
#12804=DIRECTION('center_axis',(0.,0.,-1.));
#12805=DIRECTION('ref_axis',(1.,0.,0.));
#12806=DIRECTION('center_axis',(0.,0.,1.));
#12807=DIRECTION('ref_axis',(1.,0.,0.));
#12808=DIRECTION('center_axis',(0.,0.,1.));
#12809=DIRECTION('ref_axis',(1.,0.,0.));
#12810=DIRECTION('',(0.,0.,1.));
#12811=DIRECTION('center_axis',(0.,0.,-1.));
#12812=DIRECTION('ref_axis',(1.,0.,0.));
#12813=DIRECTION('center_axis',(0.,0.,1.));
#12814=DIRECTION('ref_axis',(1.,0.,0.));
#12815=DIRECTION('center_axis',(0.,0.,1.));
#12816=DIRECTION('ref_axis',(1.,0.,0.));
#12817=DIRECTION('',(0.,0.,1.));
#12818=DIRECTION('center_axis',(0.,0.,-1.));
#12819=DIRECTION('ref_axis',(1.,0.,0.));
#12820=DIRECTION('center_axis',(0.,0.,1.));
#12821=DIRECTION('ref_axis',(1.,0.,0.));
#12822=DIRECTION('center_axis',(0.,0.,1.));
#12823=DIRECTION('ref_axis',(1.,0.,0.));
#12824=DIRECTION('',(0.,0.,1.));
#12825=DIRECTION('center_axis',(0.,0.,-1.));
#12826=DIRECTION('ref_axis',(1.,0.,0.));
#12827=DIRECTION('center_axis',(0.,0.,1.));
#12828=DIRECTION('ref_axis',(1.,0.,0.));
#12829=DIRECTION('center_axis',(0.,0.,1.));
#12830=DIRECTION('ref_axis',(1.,0.,0.));
#12831=DIRECTION('',(0.,0.,1.));
#12832=DIRECTION('center_axis',(0.,0.,-1.));
#12833=DIRECTION('ref_axis',(1.,0.,0.));
#12834=DIRECTION('center_axis',(0.,0.,1.));
#12835=DIRECTION('ref_axis',(1.,0.,0.));
#12836=DIRECTION('center_axis',(0.,0.,1.));
#12837=DIRECTION('ref_axis',(1.,0.,0.));
#12838=DIRECTION('',(0.,0.,1.));
#12839=DIRECTION('center_axis',(0.,0.,-1.));
#12840=DIRECTION('ref_axis',(1.,0.,0.));
#12841=DIRECTION('center_axis',(0.,0.,1.));
#12842=DIRECTION('ref_axis',(1.,0.,0.));
#12843=DIRECTION('center_axis',(0.,0.,1.));
#12844=DIRECTION('ref_axis',(1.,0.,0.));
#12845=DIRECTION('',(0.,0.,1.));
#12846=DIRECTION('center_axis',(0.,0.,-1.));
#12847=DIRECTION('ref_axis',(1.,0.,0.));
#12848=DIRECTION('center_axis',(0.,0.,1.));
#12849=DIRECTION('ref_axis',(1.,0.,0.));
#12850=DIRECTION('center_axis',(0.,0.,1.));
#12851=DIRECTION('ref_axis',(1.,0.,0.));
#12852=DIRECTION('',(0.,0.,1.));
#12853=DIRECTION('center_axis',(0.,0.,-1.));
#12854=DIRECTION('ref_axis',(1.,0.,0.));
#12855=DIRECTION('center_axis',(0.,0.,1.));
#12856=DIRECTION('ref_axis',(1.,0.,0.));
#12857=DIRECTION('center_axis',(0.,0.,1.));
#12858=DIRECTION('ref_axis',(1.,0.,0.));
#12859=DIRECTION('',(0.,0.,1.));
#12860=DIRECTION('center_axis',(0.,0.,-1.));
#12861=DIRECTION('ref_axis',(1.,0.,0.));
#12862=DIRECTION('center_axis',(0.,0.,1.));
#12863=DIRECTION('ref_axis',(1.,0.,0.));
#12864=DIRECTION('center_axis',(0.,0.,1.));
#12865=DIRECTION('ref_axis',(1.,0.,0.));
#12866=DIRECTION('',(0.,0.,1.));
#12867=DIRECTION('center_axis',(0.,0.,-1.));
#12868=DIRECTION('ref_axis',(1.,0.,0.));
#12869=DIRECTION('center_axis',(0.,0.,1.));
#12870=DIRECTION('ref_axis',(1.,0.,0.));
#12871=DIRECTION('center_axis',(0.,0.,1.));
#12872=DIRECTION('ref_axis',(1.,0.,0.));
#12873=DIRECTION('',(0.,0.,1.));
#12874=DIRECTION('center_axis',(0.,0.,-1.));
#12875=DIRECTION('ref_axis',(1.,0.,0.));
#12876=DIRECTION('center_axis',(0.,0.,1.));
#12877=DIRECTION('ref_axis',(1.,0.,0.));
#12878=DIRECTION('center_axis',(0.,0.,1.));
#12879=DIRECTION('ref_axis',(1.,0.,0.));
#12880=DIRECTION('',(0.,0.,1.));
#12881=DIRECTION('center_axis',(0.,0.,-1.));
#12882=DIRECTION('ref_axis',(1.,0.,0.));
#12883=DIRECTION('center_axis',(0.,0.,1.));
#12884=DIRECTION('ref_axis',(1.,0.,0.));
#12885=DIRECTION('center_axis',(0.,0.,1.));
#12886=DIRECTION('ref_axis',(1.,0.,0.));
#12887=DIRECTION('',(0.,0.,1.));
#12888=DIRECTION('center_axis',(0.,0.,-1.));
#12889=DIRECTION('ref_axis',(1.,0.,0.));
#12890=DIRECTION('center_axis',(0.,0.,1.));
#12891=DIRECTION('ref_axis',(1.,0.,0.));
#12892=DIRECTION('center_axis',(0.,0.,1.));
#12893=DIRECTION('ref_axis',(1.,0.,0.));
#12894=DIRECTION('',(0.,0.,1.));
#12895=DIRECTION('center_axis',(0.,0.,-1.));
#12896=DIRECTION('ref_axis',(1.,0.,0.));
#12897=DIRECTION('center_axis',(0.,0.,1.));
#12898=DIRECTION('ref_axis',(1.,0.,0.));
#12899=DIRECTION('center_axis',(0.,0.,1.));
#12900=DIRECTION('ref_axis',(1.,0.,0.));
#12901=DIRECTION('',(0.,0.,1.));
#12902=DIRECTION('center_axis',(0.,0.,-1.));
#12903=DIRECTION('ref_axis',(1.,0.,0.));
#12904=DIRECTION('center_axis',(0.,0.,1.));
#12905=DIRECTION('ref_axis',(1.,0.,0.));
#12906=DIRECTION('center_axis',(0.,0.,1.));
#12907=DIRECTION('ref_axis',(1.,0.,0.));
#12908=DIRECTION('',(0.,0.,1.));
#12909=DIRECTION('center_axis',(0.,0.,-1.));
#12910=DIRECTION('ref_axis',(1.,0.,0.));
#12911=DIRECTION('center_axis',(0.,0.,1.));
#12912=DIRECTION('ref_axis',(1.,0.,0.));
#12913=DIRECTION('center_axis',(0.,0.,1.));
#12914=DIRECTION('ref_axis',(1.,0.,0.));
#12915=DIRECTION('',(0.,0.,1.));
#12916=DIRECTION('center_axis',(0.,0.,-1.));
#12917=DIRECTION('ref_axis',(1.,0.,0.));
#12918=DIRECTION('center_axis',(0.,0.,1.));
#12919=DIRECTION('ref_axis',(1.,0.,0.));
#12920=DIRECTION('center_axis',(0.,0.,1.));
#12921=DIRECTION('ref_axis',(1.,0.,0.));
#12922=DIRECTION('',(0.,0.,1.));
#12923=DIRECTION('center_axis',(0.,0.,-1.));
#12924=DIRECTION('ref_axis',(1.,0.,0.));
#12925=DIRECTION('center_axis',(0.,0.,1.));
#12926=DIRECTION('ref_axis',(1.,0.,0.));
#12927=DIRECTION('center_axis',(0.,0.,1.));
#12928=DIRECTION('ref_axis',(1.,0.,0.));
#12929=DIRECTION('',(0.,0.,1.));
#12930=DIRECTION('center_axis',(0.,0.,-1.));
#12931=DIRECTION('ref_axis',(1.,0.,0.));
#12932=DIRECTION('center_axis',(0.,0.,1.));
#12933=DIRECTION('ref_axis',(1.,0.,0.));
#12934=DIRECTION('center_axis',(0.,0.,1.));
#12935=DIRECTION('ref_axis',(1.,0.,0.));
#12936=DIRECTION('',(0.,0.,1.));
#12937=DIRECTION('center_axis',(0.,0.,-1.));
#12938=DIRECTION('ref_axis',(1.,0.,0.));
#12939=DIRECTION('center_axis',(0.,1.,0.));
#12940=DIRECTION('ref_axis',(-1.,0.,0.));
#12941=DIRECTION('',(-1.,0.,0.));
#12942=DIRECTION('',(0.,0.,1.));
#12943=DIRECTION('',(-1.,0.,0.));
#12944=DIRECTION('',(0.,0.,1.));
#12945=DIRECTION('center_axis',(1.,0.,0.));
#12946=DIRECTION('ref_axis',(0.,1.,0.));
#12947=DIRECTION('',(0.,1.,0.));
#12948=DIRECTION('',(0.,1.,0.));
#12949=DIRECTION('',(0.,0.,1.));
#12950=DIRECTION('center_axis',(0.,-1.,0.));
#12951=DIRECTION('ref_axis',(1.,0.,0.));
#12952=DIRECTION('',(1.,0.,0.));
#12953=DIRECTION('',(1.,0.,0.));
#12954=DIRECTION('',(0.,0.,1.));
#12955=DIRECTION('center_axis',(-1.,0.,0.));
#12956=DIRECTION('ref_axis',(0.,-1.,0.));
#12957=DIRECTION('',(0.,-1.,0.));
#12958=DIRECTION('',(0.,-1.,0.));
#12959=DIRECTION('center_axis',(0.,0.,1.));
#12960=DIRECTION('ref_axis',(1.,0.,0.));
#12961=DIRECTION('center_axis',(0.,0.,1.));
#12962=DIRECTION('ref_axis',(1.,0.,0.));
#12963=DIRECTION('axis',(0.,0.,1.));
#12964=DIRECTION('refdir',(1.,0.,0.));
#12965=DIRECTION('center_axis',(0.,0.,1.));
#12966=DIRECTION('ref_axis',(1.,0.,0.));
#12967=DIRECTION('center_axis',(0.,0.,-1.));
#12968=DIRECTION('ref_axis',(1.,0.,0.));
#12969=DIRECTION('center_axis',(0.,0.,1.));
#12970=DIRECTION('ref_axis',(1.,0.,0.));
#12971=DIRECTION('center_axis',(0.,0.,1.));
#12972=DIRECTION('ref_axis',(1.,0.,0.));
#12973=DIRECTION('',(0.,0.,-1.));
#12974=DIRECTION('center_axis',(0.,0.,1.));
#12975=DIRECTION('ref_axis',(1.,0.,0.));
#12976=DIRECTION('',(0.,0.,1.));
#12977=DIRECTION('center_axis',(0.,0.,-1.));
#12978=DIRECTION('ref_axis',(1.,0.,0.));
#12979=DIRECTION('center_axis',(0.,0.,1.));
#12980=DIRECTION('ref_axis',(1.,0.,0.));
#12981=DIRECTION('',(0.,0.,1.));
#12982=DIRECTION('center_axis',(0.,0.,1.));
#12983=DIRECTION('ref_axis',(1.,0.,0.));
#12984=DIRECTION('center_axis',(0.,0.,-1.));
#12985=DIRECTION('ref_axis',(1.,0.,0.));
#12986=DIRECTION('center_axis',(0.,0.,1.));
#12987=DIRECTION('ref_axis',(1.,0.,0.));
#12988=DIRECTION('center_axis',(0.,0.,1.));
#12989=DIRECTION('ref_axis',(1.,0.,0.));
#12990=DIRECTION('',(0.,0.,-1.));
#12991=DIRECTION('center_axis',(0.,0.,1.));
#12992=DIRECTION('ref_axis',(1.,0.,0.));
#12993=DIRECTION('',(0.,0.,1.));
#12994=DIRECTION('center_axis',(0.,0.,-1.));
#12995=DIRECTION('ref_axis',(1.,0.,0.));
#12996=DIRECTION('center_axis',(0.,0.,1.));
#12997=DIRECTION('ref_axis',(1.,0.,0.));
#12998=DIRECTION('',(0.,0.,1.));
#12999=DIRECTION('center_axis',(0.,0.,1.));
#13000=DIRECTION('ref_axis',(1.,0.,0.));
#13001=DIRECTION('center_axis',(0.,0.,-1.));
#13002=DIRECTION('ref_axis',(1.,0.,0.));
#13003=DIRECTION('center_axis',(0.,0.,1.));
#13004=DIRECTION('ref_axis',(1.,0.,0.));
#13005=DIRECTION('center_axis',(0.,0.,1.));
#13006=DIRECTION('ref_axis',(1.,0.,0.));
#13007=DIRECTION('center_axis',(0.,0.,1.));
#13008=DIRECTION('ref_axis',(1.,0.,0.));
#13009=DIRECTION('',(0.,0.,-1.));
#13010=DIRECTION('center_axis',(0.,0.,1.));
#13011=DIRECTION('ref_axis',(1.,0.,0.));
#13012=DIRECTION('',(0.,0.,1.));
#13013=DIRECTION('',(0.,0.,1.));
#13014=DIRECTION('center_axis',(0.,0.,-1.));
#13015=DIRECTION('ref_axis',(1.,0.,0.));
#13016=DIRECTION('center_axis',(0.,0.,1.));
#13017=DIRECTION('ref_axis',(1.,0.,0.));
#13018=DIRECTION('center_axis',(0.,0.,-1.));
#13019=DIRECTION('ref_axis',(1.,0.,0.));
#13020=DIRECTION('center_axis',(0.,0.,1.));
#13021=DIRECTION('ref_axis',(1.,0.,0.));
#13022=DIRECTION('center_axis',(0.,0.,1.));
#13023=DIRECTION('ref_axis',(1.,0.,0.));
#13024=DIRECTION('center_axis',(0.,0.,1.));
#13025=DIRECTION('ref_axis',(1.,0.,0.));
#13026=DIRECTION('',(0.,0.,-1.));
#13027=DIRECTION('center_axis',(0.,0.,1.));
#13028=DIRECTION('ref_axis',(1.,0.,0.));
#13029=DIRECTION('',(0.,0.,1.));
#13030=DIRECTION('',(0.,0.,1.));
#13031=DIRECTION('center_axis',(0.,0.,-1.));
#13032=DIRECTION('ref_axis',(1.,0.,0.));
#13033=DIRECTION('center_axis',(0.,0.,1.));
#13034=DIRECTION('ref_axis',(1.,0.,0.));
#13035=DIRECTION('center_axis',(0.,0.,-1.));
#13036=DIRECTION('ref_axis',(1.,0.,0.));
#13037=DIRECTION('',(0.,0.,-1.));
#13038=DIRECTION('center_axis',(0.,0.,1.));
#13039=DIRECTION('ref_axis',(1.,0.,0.));
#13040=DIRECTION('center_axis',(0.,0.,-1.));
#13041=DIRECTION('ref_axis',(1.,0.,0.));
#13042=DIRECTION('center_axis',(0.,0.,-1.));
#13043=DIRECTION('ref_axis',(1.,0.,0.));
#13044=DIRECTION('center_axis',(0.,0.,-1.));
#13045=DIRECTION('ref_axis',(1.,0.,0.));
#13046=DIRECTION('center_axis',(0.,0.,-1.));
#13047=DIRECTION('ref_axis',(1.,0.,0.));
#13048=DIRECTION('center_axis',(0.,0.,1.));
#13049=DIRECTION('ref_axis',(1.,0.,0.));
#13050=DIRECTION('center_axis',(0.,0.,1.));
#13051=DIRECTION('ref_axis',(1.,0.,0.));
#13052=DIRECTION('',(0.,0.,1.));
#13053=DIRECTION('center_axis',(0.,0.,-1.));
#13054=DIRECTION('ref_axis',(1.,0.,0.));
#13055=DIRECTION('center_axis',(0.,0.,1.));
#13056=DIRECTION('ref_axis',(1.,0.,0.));
#13057=DIRECTION('center_axis',(0.,0.,1.));
#13058=DIRECTION('ref_axis',(1.,0.,0.));
#13059=DIRECTION('center_axis',(0.,0.,1.));
#13060=DIRECTION('ref_axis',(1.,0.,0.));
#13061=DIRECTION('center_axis',(0.,0.,1.));
#13062=DIRECTION('ref_axis',(1.,0.,0.));
#13063=DIRECTION('center_axis',(0.,0.,1.));
#13064=DIRECTION('ref_axis',(1.,0.,0.));
#13065=DIRECTION('center_axis',(0.,0.,1.));
#13066=DIRECTION('ref_axis',(1.,0.,0.));
#13067=DIRECTION('',(0.,0.,-1.));
#13068=DIRECTION('center_axis',(0.,0.,1.));
#13069=DIRECTION('ref_axis',(1.,0.,0.));
#13070=DIRECTION('',(0.,0.,-1.));
#13071=DIRECTION('center_axis',(0.,0.,-1.));
#13072=DIRECTION('ref_axis',(1.,0.,0.));
#13073=DIRECTION('center_axis',(0.,0.,1.));
#13074=DIRECTION('ref_axis',(1.,0.,0.));
#13075=DIRECTION('center_axis',(0.,0.,1.));
#13076=DIRECTION('ref_axis',(1.,0.,0.));
#13077=DIRECTION('axis',(0.,0.,1.));
#13078=DIRECTION('refdir',(1.,0.,0.));
#13079=DIRECTION('center_axis',(0.,0.,1.));
#13080=DIRECTION('ref_axis',(1.,0.,0.));
#13081=DIRECTION('center_axis',(0.,0.,-1.));
#13082=DIRECTION('ref_axis',(1.,0.,0.));
#13083=DIRECTION('center_axis',(0.,0.,1.));
#13084=DIRECTION('ref_axis',(1.,0.,0.));
#13085=DIRECTION('center_axis',(0.,0.,1.));
#13086=DIRECTION('ref_axis',(1.,0.,0.));
#13087=DIRECTION('',(0.,0.,-1.));
#13088=DIRECTION('center_axis',(0.,0.,1.));
#13089=DIRECTION('ref_axis',(1.,0.,0.));
#13090=DIRECTION('',(0.,0.,1.));
#13091=DIRECTION('center_axis',(0.,0.,-1.));
#13092=DIRECTION('ref_axis',(1.,0.,0.));
#13093=DIRECTION('center_axis',(0.,0.,1.));
#13094=DIRECTION('ref_axis',(1.,0.,0.));
#13095=DIRECTION('',(0.,0.,1.));
#13096=DIRECTION('center_axis',(0.,0.,1.));
#13097=DIRECTION('ref_axis',(1.,0.,0.));
#13098=DIRECTION('center_axis',(0.,0.,-1.));
#13099=DIRECTION('ref_axis',(1.,0.,0.));
#13100=DIRECTION('center_axis',(0.,0.,1.));
#13101=DIRECTION('ref_axis',(1.,0.,0.));
#13102=DIRECTION('center_axis',(0.,0.,1.));
#13103=DIRECTION('ref_axis',(1.,0.,0.));
#13104=DIRECTION('',(0.,0.,-1.));
#13105=DIRECTION('center_axis',(0.,0.,1.));
#13106=DIRECTION('ref_axis',(1.,0.,0.));
#13107=DIRECTION('',(0.,0.,1.));
#13108=DIRECTION('center_axis',(0.,0.,-1.));
#13109=DIRECTION('ref_axis',(1.,0.,0.));
#13110=DIRECTION('center_axis',(0.,0.,1.));
#13111=DIRECTION('ref_axis',(1.,0.,0.));
#13112=DIRECTION('',(0.,0.,1.));
#13113=DIRECTION('center_axis',(0.,0.,1.));
#13114=DIRECTION('ref_axis',(1.,0.,0.));
#13115=DIRECTION('center_axis',(0.,0.,-1.));
#13116=DIRECTION('ref_axis',(1.,0.,0.));
#13117=DIRECTION('center_axis',(0.,0.,1.));
#13118=DIRECTION('ref_axis',(1.,0.,0.));
#13119=DIRECTION('center_axis',(0.,0.,1.));
#13120=DIRECTION('ref_axis',(1.,0.,0.));
#13121=DIRECTION('center_axis',(0.,0.,1.));
#13122=DIRECTION('ref_axis',(1.,0.,0.));
#13123=DIRECTION('',(0.,0.,-1.));
#13124=DIRECTION('center_axis',(0.,0.,1.));
#13125=DIRECTION('ref_axis',(1.,0.,0.));
#13126=DIRECTION('',(0.,0.,1.));
#13127=DIRECTION('',(0.,0.,1.));
#13128=DIRECTION('center_axis',(0.,0.,-1.));
#13129=DIRECTION('ref_axis',(1.,0.,0.));
#13130=DIRECTION('center_axis',(0.,0.,1.));
#13131=DIRECTION('ref_axis',(1.,0.,0.));
#13132=DIRECTION('center_axis',(0.,0.,-1.));
#13133=DIRECTION('ref_axis',(1.,0.,0.));
#13134=DIRECTION('center_axis',(0.,0.,1.));
#13135=DIRECTION('ref_axis',(1.,0.,0.));
#13136=DIRECTION('center_axis',(0.,0.,1.));
#13137=DIRECTION('ref_axis',(1.,0.,0.));
#13138=DIRECTION('center_axis',(0.,0.,1.));
#13139=DIRECTION('ref_axis',(1.,0.,0.));
#13140=DIRECTION('',(0.,0.,-1.));
#13141=DIRECTION('center_axis',(0.,0.,1.));
#13142=DIRECTION('ref_axis',(1.,0.,0.));
#13143=DIRECTION('',(0.,0.,1.));
#13144=DIRECTION('',(0.,0.,1.));
#13145=DIRECTION('center_axis',(0.,0.,-1.));
#13146=DIRECTION('ref_axis',(1.,0.,0.));
#13147=DIRECTION('center_axis',(0.,0.,1.));
#13148=DIRECTION('ref_axis',(1.,0.,0.));
#13149=DIRECTION('center_axis',(0.,0.,-1.));
#13150=DIRECTION('ref_axis',(1.,0.,0.));
#13151=DIRECTION('',(0.,0.,-1.));
#13152=DIRECTION('center_axis',(0.,0.,1.));
#13153=DIRECTION('ref_axis',(1.,0.,0.));
#13154=DIRECTION('center_axis',(0.,0.,-1.));
#13155=DIRECTION('ref_axis',(1.,0.,0.));
#13156=DIRECTION('center_axis',(0.,0.,-1.));
#13157=DIRECTION('ref_axis',(1.,0.,0.));
#13158=DIRECTION('center_axis',(0.,0.,-1.));
#13159=DIRECTION('ref_axis',(1.,0.,0.));
#13160=DIRECTION('center_axis',(0.,0.,-1.));
#13161=DIRECTION('ref_axis',(1.,0.,0.));
#13162=DIRECTION('center_axis',(0.,0.,1.));
#13163=DIRECTION('ref_axis',(1.,0.,0.));
#13164=DIRECTION('center_axis',(0.,0.,1.));
#13165=DIRECTION('ref_axis',(1.,0.,0.));
#13166=DIRECTION('',(0.,0.,1.));
#13167=DIRECTION('center_axis',(0.,0.,-1.));
#13168=DIRECTION('ref_axis',(1.,0.,0.));
#13169=DIRECTION('center_axis',(0.,0.,1.));
#13170=DIRECTION('ref_axis',(1.,0.,0.));
#13171=DIRECTION('center_axis',(0.,0.,1.));
#13172=DIRECTION('ref_axis',(1.,0.,0.));
#13173=DIRECTION('center_axis',(0.,0.,1.));
#13174=DIRECTION('ref_axis',(1.,0.,0.));
#13175=DIRECTION('center_axis',(0.,0.,1.));
#13176=DIRECTION('ref_axis',(1.,0.,0.));
#13177=DIRECTION('center_axis',(0.,0.,1.));
#13178=DIRECTION('ref_axis',(1.,0.,0.));
#13179=DIRECTION('center_axis',(0.,0.,1.));
#13180=DIRECTION('ref_axis',(1.,0.,0.));
#13181=DIRECTION('',(0.,0.,-1.));
#13182=DIRECTION('center_axis',(0.,0.,1.));
#13183=DIRECTION('ref_axis',(1.,0.,0.));
#13184=DIRECTION('',(0.,0.,-1.));
#13185=DIRECTION('center_axis',(0.,0.,-1.));
#13186=DIRECTION('ref_axis',(1.,0.,0.));
#13187=DIRECTION('center_axis',(0.,0.,1.));
#13188=DIRECTION('ref_axis',(1.,0.,0.));
#13189=DIRECTION('center_axis',(0.,0.,1.));
#13190=DIRECTION('ref_axis',(1.,0.,0.));
#13191=DIRECTION('axis',(0.,0.,1.));
#13192=DIRECTION('refdir',(1.,0.,0.));
#13193=DIRECTION('center_axis',(0.,0.,1.));
#13194=DIRECTION('ref_axis',(1.,0.,0.));
#13195=DIRECTION('center_axis',(0.,0.,-1.));
#13196=DIRECTION('ref_axis',(1.,0.,0.));
#13197=DIRECTION('center_axis',(0.,0.,1.));
#13198=DIRECTION('ref_axis',(1.,0.,0.));
#13199=DIRECTION('center_axis',(0.,0.,1.));
#13200=DIRECTION('ref_axis',(1.,0.,0.));
#13201=DIRECTION('',(0.,0.,-1.));
#13202=DIRECTION('center_axis',(0.,0.,1.));
#13203=DIRECTION('ref_axis',(1.,0.,0.));
#13204=DIRECTION('',(0.,0.,1.));
#13205=DIRECTION('center_axis',(0.,0.,-1.));
#13206=DIRECTION('ref_axis',(1.,0.,0.));
#13207=DIRECTION('center_axis',(0.,0.,1.));
#13208=DIRECTION('ref_axis',(1.,0.,0.));
#13209=DIRECTION('',(0.,0.,1.));
#13210=DIRECTION('center_axis',(0.,0.,1.));
#13211=DIRECTION('ref_axis',(1.,0.,0.));
#13212=DIRECTION('center_axis',(0.,0.,-1.));
#13213=DIRECTION('ref_axis',(1.,0.,0.));
#13214=DIRECTION('center_axis',(0.,0.,1.));
#13215=DIRECTION('ref_axis',(1.,0.,0.));
#13216=DIRECTION('center_axis',(0.,0.,1.));
#13217=DIRECTION('ref_axis',(1.,0.,0.));
#13218=DIRECTION('',(0.,0.,-1.));
#13219=DIRECTION('center_axis',(0.,0.,1.));
#13220=DIRECTION('ref_axis',(1.,0.,0.));
#13221=DIRECTION('',(0.,0.,1.));
#13222=DIRECTION('center_axis',(0.,0.,-1.));
#13223=DIRECTION('ref_axis',(1.,0.,0.));
#13224=DIRECTION('center_axis',(0.,0.,1.));
#13225=DIRECTION('ref_axis',(1.,0.,0.));
#13226=DIRECTION('',(0.,0.,1.));
#13227=DIRECTION('center_axis',(0.,0.,1.));
#13228=DIRECTION('ref_axis',(1.,0.,0.));
#13229=DIRECTION('center_axis',(0.,0.,-1.));
#13230=DIRECTION('ref_axis',(1.,0.,0.));
#13231=DIRECTION('center_axis',(0.,0.,1.));
#13232=DIRECTION('ref_axis',(1.,0.,0.));
#13233=DIRECTION('center_axis',(0.,0.,1.));
#13234=DIRECTION('ref_axis',(1.,0.,0.));
#13235=DIRECTION('center_axis',(0.,0.,1.));
#13236=DIRECTION('ref_axis',(1.,0.,0.));
#13237=DIRECTION('',(0.,0.,-1.));
#13238=DIRECTION('center_axis',(0.,0.,1.));
#13239=DIRECTION('ref_axis',(1.,0.,0.));
#13240=DIRECTION('',(0.,0.,1.));
#13241=DIRECTION('',(0.,0.,1.));
#13242=DIRECTION('center_axis',(0.,0.,-1.));
#13243=DIRECTION('ref_axis',(1.,0.,0.));
#13244=DIRECTION('center_axis',(0.,0.,1.));
#13245=DIRECTION('ref_axis',(1.,0.,0.));
#13246=DIRECTION('center_axis',(0.,0.,-1.));
#13247=DIRECTION('ref_axis',(1.,0.,0.));
#13248=DIRECTION('center_axis',(0.,0.,1.));
#13249=DIRECTION('ref_axis',(1.,0.,0.));
#13250=DIRECTION('center_axis',(0.,0.,1.));
#13251=DIRECTION('ref_axis',(1.,0.,0.));
#13252=DIRECTION('center_axis',(0.,0.,1.));
#13253=DIRECTION('ref_axis',(1.,0.,0.));
#13254=DIRECTION('',(0.,0.,-1.));
#13255=DIRECTION('center_axis',(0.,0.,1.));
#13256=DIRECTION('ref_axis',(1.,0.,0.));
#13257=DIRECTION('',(0.,0.,1.));
#13258=DIRECTION('',(0.,0.,1.));
#13259=DIRECTION('center_axis',(0.,0.,-1.));
#13260=DIRECTION('ref_axis',(1.,0.,0.));
#13261=DIRECTION('center_axis',(0.,0.,1.));
#13262=DIRECTION('ref_axis',(1.,0.,0.));
#13263=DIRECTION('center_axis',(0.,0.,-1.));
#13264=DIRECTION('ref_axis',(1.,0.,0.));
#13265=DIRECTION('',(0.,0.,-1.));
#13266=DIRECTION('center_axis',(0.,0.,1.));
#13267=DIRECTION('ref_axis',(1.,0.,0.));
#13268=DIRECTION('center_axis',(0.,0.,-1.));
#13269=DIRECTION('ref_axis',(1.,0.,0.));
#13270=DIRECTION('center_axis',(0.,0.,-1.));
#13271=DIRECTION('ref_axis',(1.,0.,0.));
#13272=DIRECTION('center_axis',(0.,0.,-1.));
#13273=DIRECTION('ref_axis',(1.,0.,0.));
#13274=DIRECTION('center_axis',(0.,0.,-1.));
#13275=DIRECTION('ref_axis',(1.,0.,0.));
#13276=DIRECTION('center_axis',(0.,0.,1.));
#13277=DIRECTION('ref_axis',(1.,0.,0.));
#13278=DIRECTION('center_axis',(0.,0.,1.));
#13279=DIRECTION('ref_axis',(1.,0.,0.));
#13280=DIRECTION('',(0.,0.,1.));
#13281=DIRECTION('center_axis',(0.,0.,-1.));
#13282=DIRECTION('ref_axis',(1.,0.,0.));
#13283=DIRECTION('center_axis',(0.,0.,1.));
#13284=DIRECTION('ref_axis',(1.,0.,0.));
#13285=DIRECTION('center_axis',(0.,0.,1.));
#13286=DIRECTION('ref_axis',(1.,0.,0.));
#13287=DIRECTION('center_axis',(0.,0.,1.));
#13288=DIRECTION('ref_axis',(1.,0.,0.));
#13289=DIRECTION('center_axis',(0.,0.,1.));
#13290=DIRECTION('ref_axis',(1.,0.,0.));
#13291=DIRECTION('center_axis',(0.,0.,1.));
#13292=DIRECTION('ref_axis',(1.,0.,0.));
#13293=DIRECTION('center_axis',(0.,0.,1.));
#13294=DIRECTION('ref_axis',(1.,0.,0.));
#13295=DIRECTION('',(0.,0.,-1.));
#13296=DIRECTION('center_axis',(0.,0.,1.));
#13297=DIRECTION('ref_axis',(1.,0.,0.));
#13298=DIRECTION('',(0.,0.,-1.));
#13299=DIRECTION('center_axis',(0.,0.,-1.));
#13300=DIRECTION('ref_axis',(1.,0.,0.));
#13301=DIRECTION('center_axis',(0.,0.,1.));
#13302=DIRECTION('ref_axis',(1.,0.,0.));
#13303=DIRECTION('center_axis',(0.,0.,1.));
#13304=DIRECTION('ref_axis',(1.,0.,0.));
#13305=DIRECTION('axis',(0.,0.,1.));
#13306=DIRECTION('refdir',(1.,0.,0.));
#13307=DIRECTION('center_axis',(0.,0.,1.));
#13308=DIRECTION('ref_axis',(1.,0.,0.));
#13309=DIRECTION('center_axis',(0.,0.,-1.));
#13310=DIRECTION('ref_axis',(1.,0.,0.));
#13311=DIRECTION('center_axis',(0.,0.,1.));
#13312=DIRECTION('ref_axis',(1.,0.,0.));
#13313=DIRECTION('center_axis',(0.,0.,1.));
#13314=DIRECTION('ref_axis',(1.,0.,0.));
#13315=DIRECTION('',(0.,0.,-1.));
#13316=DIRECTION('center_axis',(0.,0.,1.));
#13317=DIRECTION('ref_axis',(1.,0.,0.));
#13318=DIRECTION('',(0.,0.,1.));
#13319=DIRECTION('center_axis',(0.,0.,-1.));
#13320=DIRECTION('ref_axis',(1.,0.,0.));
#13321=DIRECTION('center_axis',(0.,0.,1.));
#13322=DIRECTION('ref_axis',(1.,0.,0.));
#13323=DIRECTION('',(0.,0.,1.));
#13324=DIRECTION('center_axis',(0.,0.,1.));
#13325=DIRECTION('ref_axis',(1.,0.,0.));
#13326=DIRECTION('center_axis',(0.,0.,-1.));
#13327=DIRECTION('ref_axis',(1.,0.,0.));
#13328=DIRECTION('center_axis',(0.,0.,1.));
#13329=DIRECTION('ref_axis',(1.,0.,0.));
#13330=DIRECTION('center_axis',(0.,0.,1.));
#13331=DIRECTION('ref_axis',(1.,0.,0.));
#13332=DIRECTION('',(0.,0.,-1.));
#13333=DIRECTION('center_axis',(0.,0.,1.));
#13334=DIRECTION('ref_axis',(1.,0.,0.));
#13335=DIRECTION('',(0.,0.,1.));
#13336=DIRECTION('center_axis',(0.,0.,-1.));
#13337=DIRECTION('ref_axis',(1.,0.,0.));
#13338=DIRECTION('center_axis',(0.,0.,1.));
#13339=DIRECTION('ref_axis',(1.,0.,0.));
#13340=DIRECTION('',(0.,0.,1.));
#13341=DIRECTION('center_axis',(0.,0.,1.));
#13342=DIRECTION('ref_axis',(1.,0.,0.));
#13343=DIRECTION('center_axis',(0.,0.,-1.));
#13344=DIRECTION('ref_axis',(1.,0.,0.));
#13345=DIRECTION('center_axis',(0.,0.,1.));
#13346=DIRECTION('ref_axis',(1.,0.,0.));
#13347=DIRECTION('center_axis',(0.,0.,1.));
#13348=DIRECTION('ref_axis',(1.,0.,0.));
#13349=DIRECTION('center_axis',(0.,0.,1.));
#13350=DIRECTION('ref_axis',(1.,0.,0.));
#13351=DIRECTION('',(0.,0.,-1.));
#13352=DIRECTION('center_axis',(0.,0.,1.));
#13353=DIRECTION('ref_axis',(1.,0.,0.));
#13354=DIRECTION('',(0.,0.,1.));
#13355=DIRECTION('',(0.,0.,1.));
#13356=DIRECTION('center_axis',(0.,0.,-1.));
#13357=DIRECTION('ref_axis',(1.,0.,0.));
#13358=DIRECTION('center_axis',(0.,0.,1.));
#13359=DIRECTION('ref_axis',(1.,0.,0.));
#13360=DIRECTION('center_axis',(0.,0.,-1.));
#13361=DIRECTION('ref_axis',(1.,0.,0.));
#13362=DIRECTION('center_axis',(0.,0.,1.));
#13363=DIRECTION('ref_axis',(1.,0.,0.));
#13364=DIRECTION('center_axis',(0.,0.,1.));
#13365=DIRECTION('ref_axis',(1.,0.,0.));
#13366=DIRECTION('center_axis',(0.,0.,1.));
#13367=DIRECTION('ref_axis',(1.,0.,0.));
#13368=DIRECTION('',(0.,0.,-1.));
#13369=DIRECTION('center_axis',(0.,0.,1.));
#13370=DIRECTION('ref_axis',(1.,0.,0.));
#13371=DIRECTION('',(0.,0.,1.));
#13372=DIRECTION('',(0.,0.,1.));
#13373=DIRECTION('center_axis',(0.,0.,-1.));
#13374=DIRECTION('ref_axis',(1.,0.,0.));
#13375=DIRECTION('center_axis',(0.,0.,1.));
#13376=DIRECTION('ref_axis',(1.,0.,0.));
#13377=DIRECTION('center_axis',(0.,0.,-1.));
#13378=DIRECTION('ref_axis',(1.,0.,0.));
#13379=DIRECTION('',(0.,0.,-1.));
#13380=DIRECTION('center_axis',(0.,0.,1.));
#13381=DIRECTION('ref_axis',(1.,0.,0.));
#13382=DIRECTION('center_axis',(0.,0.,-1.));
#13383=DIRECTION('ref_axis',(1.,0.,0.));
#13384=DIRECTION('center_axis',(0.,0.,-1.));
#13385=DIRECTION('ref_axis',(1.,0.,0.));
#13386=DIRECTION('center_axis',(0.,0.,-1.));
#13387=DIRECTION('ref_axis',(1.,0.,0.));
#13388=DIRECTION('center_axis',(0.,0.,-1.));
#13389=DIRECTION('ref_axis',(1.,0.,0.));
#13390=DIRECTION('center_axis',(0.,0.,1.));
#13391=DIRECTION('ref_axis',(1.,0.,0.));
#13392=DIRECTION('center_axis',(0.,0.,1.));
#13393=DIRECTION('ref_axis',(1.,0.,0.));
#13394=DIRECTION('',(0.,0.,1.));
#13395=DIRECTION('center_axis',(0.,0.,-1.));
#13396=DIRECTION('ref_axis',(1.,0.,0.));
#13397=DIRECTION('center_axis',(0.,0.,1.));
#13398=DIRECTION('ref_axis',(1.,0.,0.));
#13399=DIRECTION('center_axis',(0.,0.,1.));
#13400=DIRECTION('ref_axis',(1.,0.,0.));
#13401=DIRECTION('center_axis',(0.,0.,1.));
#13402=DIRECTION('ref_axis',(1.,0.,0.));
#13403=DIRECTION('center_axis',(0.,0.,1.));
#13404=DIRECTION('ref_axis',(1.,0.,0.));
#13405=DIRECTION('center_axis',(0.,0.,1.));
#13406=DIRECTION('ref_axis',(1.,0.,0.));
#13407=DIRECTION('center_axis',(0.,0.,1.));
#13408=DIRECTION('ref_axis',(1.,0.,0.));
#13409=DIRECTION('',(0.,0.,-1.));
#13410=DIRECTION('center_axis',(0.,0.,1.));
#13411=DIRECTION('ref_axis',(1.,0.,0.));
#13412=DIRECTION('',(0.,0.,-1.));
#13413=DIRECTION('center_axis',(0.,0.,-1.));
#13414=DIRECTION('ref_axis',(1.,0.,0.));
#13415=DIRECTION('center_axis',(0.,0.,1.));
#13416=DIRECTION('ref_axis',(1.,0.,0.));
#13417=DIRECTION('center_axis',(0.,0.,1.));
#13418=DIRECTION('ref_axis',(1.,0.,0.));
#13419=DIRECTION('axis',(0.,0.,1.));
#13420=DIRECTION('refdir',(1.,0.,0.));
#13421=DIRECTION('center_axis',(0.,0.,1.));
#13422=DIRECTION('ref_axis',(1.,0.,0.));
#13423=DIRECTION('center_axis',(0.,0.,1.));
#13424=DIRECTION('ref_axis',(1.,0.,0.));
#13425=DIRECTION('',(0.,0.,1.));
#13426=DIRECTION('center_axis',(0.,0.,-1.));
#13427=DIRECTION('ref_axis',(1.,0.,0.));
#13428=DIRECTION('center_axis',(0.,0.,1.));
#13429=DIRECTION('ref_axis',(1.,0.,0.));
#13430=DIRECTION('center_axis',(0.,0.,1.));
#13431=DIRECTION('ref_axis',(1.,0.,0.));
#13432=DIRECTION('',(0.,0.,1.));
#13433=DIRECTION('center_axis',(0.,0.,-1.));
#13434=DIRECTION('ref_axis',(1.,0.,0.));
#13435=DIRECTION('center_axis',(0.,0.,1.));
#13436=DIRECTION('ref_axis',(1.,0.,0.));
#13437=DIRECTION('center_axis',(0.,0.,1.));
#13438=DIRECTION('ref_axis',(1.,0.,0.));
#13439=DIRECTION('',(0.,0.,1.));
#13440=DIRECTION('center_axis',(0.,0.,-1.));
#13441=DIRECTION('ref_axis',(1.,0.,0.));
#13442=DIRECTION('center_axis',(0.,0.,1.));
#13443=DIRECTION('ref_axis',(1.,0.,0.));
#13444=DIRECTION('center_axis',(0.,0.,1.));
#13445=DIRECTION('ref_axis',(1.,0.,0.));
#13446=DIRECTION('',(0.,0.,1.));
#13447=DIRECTION('center_axis',(0.,0.,-1.));
#13448=DIRECTION('ref_axis',(1.,0.,0.));
#13449=DIRECTION('center_axis',(0.,0.,1.));
#13450=DIRECTION('ref_axis',(1.,0.,0.));
#13451=DIRECTION('center_axis',(0.,0.,1.));
#13452=DIRECTION('ref_axis',(1.,0.,0.));
#13453=DIRECTION('center_axis',(0.,0.,-1.));
#13454=DIRECTION('ref_axis',(1.,0.,0.));
#13455=DIRECTION('center_axis',(0.,0.,1.));
#13456=DIRECTION('ref_axis',(1.,0.,0.));
#13457=DIRECTION('center_axis',(0.,0.,1.));
#13458=DIRECTION('ref_axis',(1.,0.,0.));
#13459=DIRECTION('',(0.,0.,-1.));
#13460=DIRECTION('center_axis',(0.,0.,1.));
#13461=DIRECTION('ref_axis',(1.,0.,0.));
#13462=DIRECTION('',(0.,0.,-1.));
#13463=DIRECTION('center_axis',(0.,0.,1.));
#13464=DIRECTION('ref_axis',(1.,0.,0.));
#13465=DIRECTION('center_axis',(0.,0.,1.));
#13466=DIRECTION('ref_axis',(1.,0.,0.));
#13467=DIRECTION('center_axis',(0.,0.,1.));
#13468=DIRECTION('ref_axis',(1.,0.,0.));
#13469=DIRECTION('axis',(0.,0.,1.));
#13470=DIRECTION('refdir',(1.,0.,0.));
#13471=DIRECTION('axis',(0.,0.,1.));
#13472=DIRECTION('refdir',(1.,0.,0.));
#13473=DIRECTION('center_axis',(0.,1.,0.));
#13474=DIRECTION('ref_axis',(0.,0.,1.));
#13475=DIRECTION('center_axis',(0.,-1.,0.));
#13476=DIRECTION('ref_axis',(1.,0.,0.));
#13477=DIRECTION('',(-1.,0.,0.));
#13478=DIRECTION('',(0.,0.,-1.));
#13479=DIRECTION('',(1.,0.,0.));
#13480=DIRECTION('center_axis',(0.,0.,1.));
#13481=DIRECTION('ref_axis',(1.,0.,0.));
#13482=DIRECTION('',(0.,-1.,0.));
#13483=DIRECTION('',(0.,1.,0.));
#13484=DIRECTION('',(-1.,0.,0.));
#13485=DIRECTION('center_axis',(0.,-1.,0.));
#13486=DIRECTION('ref_axis',(0.,0.,-1.));
#13487=DIRECTION('center_axis',(0.,1.,0.));
#13488=DIRECTION('ref_axis',(1.,0.,0.));
#13489=DIRECTION('',(0.,0.,1.));
#13490=DIRECTION('',(1.,0.,0.));
#13491=DIRECTION('center_axis',(0.,0.,-1.));
#13492=DIRECTION('ref_axis',(-1.,0.,0.));
#13493=DIRECTION('',(0.,1.,0.));
#13494=DIRECTION('',(0.,1.,0.));
#13495=DIRECTION('center_axis',(1.,0.,0.));
#13496=DIRECTION('ref_axis',(0.,0.,-1.));
#13497=DIRECTION('center_axis',(0.,1.,0.));
#13498=DIRECTION('ref_axis',(0.,0.,1.));
#13499=DIRECTION('center_axis',(0.,-1.,0.));
#13500=DIRECTION('ref_axis',(1.,0.,0.));
#13501=DIRECTION('center_axis',(0.,-1.,0.));
#13502=DIRECTION('ref_axis',(1.,0.,0.));
#13503=DIRECTION('center_axis',(0.,-1.,0.));
#13504=DIRECTION('ref_axis',(1.,0.,0.));
#13505=DIRECTION('center_axis',(0.,-1.,0.));
#13506=DIRECTION('ref_axis',(1.,0.,0.));
#13507=DIRECTION('',(0.,1.,0.));
#13508=DIRECTION('center_axis',(0.,-1.,0.));
#13509=DIRECTION('ref_axis',(0.,0.,-1.));
#13510=DIRECTION('center_axis',(0.,-1.,0.));
#13511=DIRECTION('ref_axis',(1.,0.,0.));
#13512=DIRECTION('center_axis',(0.,-1.,0.));
#13513=DIRECTION('ref_axis',(1.,0.,0.));
#13514=DIRECTION('center_axis',(0.,-1.,0.));
#13515=DIRECTION('ref_axis',(1.,0.,0.));
#13516=DIRECTION('',(0.,1.,0.));
#13517=DIRECTION('center_axis',(0.,1.,0.));
#13518=DIRECTION('ref_axis',(0.,0.,1.));
#13519=DIRECTION('center_axis',(0.,-1.,0.));
#13520=DIRECTION('ref_axis',(1.,0.,0.));
#13521=DIRECTION('center_axis',(0.,-1.,0.));
#13522=DIRECTION('ref_axis',(1.,0.,0.));
#13523=DIRECTION('center_axis',(0.,-1.,0.));
#13524=DIRECTION('ref_axis',(1.,0.,0.));
#13525=DIRECTION('',(0.,1.,0.));
#13526=DIRECTION('center_axis',(0.,-1.,0.));
#13527=DIRECTION('ref_axis',(0.,0.,-1.));
#13528=DIRECTION('center_axis',(0.,-1.,0.));
#13529=DIRECTION('ref_axis',(1.,0.,0.));
#13530=DIRECTION('center_axis',(0.,-1.,0.));
#13531=DIRECTION('ref_axis',(1.,0.,0.));
#13532=DIRECTION('center_axis',(0.,-1.,0.));
#13533=DIRECTION('ref_axis',(1.,0.,0.));
#13534=DIRECTION('',(0.,1.,0.));
#13535=DIRECTION('center_axis',(0.,1.,0.));
#13536=DIRECTION('ref_axis',(0.,0.,1.));
#13537=DIRECTION('center_axis',(0.,-1.,0.));
#13538=DIRECTION('ref_axis',(1.,0.,0.));
#13539=DIRECTION('center_axis',(0.,-1.,0.));
#13540=DIRECTION('ref_axis',(1.,0.,0.));
#13541=DIRECTION('center_axis',(0.,-1.,0.));
#13542=DIRECTION('ref_axis',(1.,0.,0.));
#13543=DIRECTION('',(0.,1.,0.));
#13544=DIRECTION('center_axis',(0.,-1.,0.));
#13545=DIRECTION('ref_axis',(0.,0.,-1.));
#13546=DIRECTION('center_axis',(0.,-1.,0.));
#13547=DIRECTION('ref_axis',(1.,0.,0.));
#13548=DIRECTION('center_axis',(0.,-1.,0.));
#13549=DIRECTION('ref_axis',(1.,0.,0.));
#13550=DIRECTION('',(0.,1.,0.));
#13551=DIRECTION('axis',(0.,0.,1.));
#13552=DIRECTION('refdir',(1.,0.,0.));
#13553=DIRECTION('center_axis',(0.,1.,0.));
#13554=DIRECTION('ref_axis',(0.,0.,1.));
#13555=DIRECTION('center_axis',(0.,1.,0.));
#13556=DIRECTION('ref_axis',(1.,0.,0.));
#13557=DIRECTION('',(1.,0.,0.));
#13558=DIRECTION('center_axis',(0.,-1.,0.));
#13559=DIRECTION('ref_axis',(1.,0.,0.));
#13560=DIRECTION('',(-1.,0.,0.));
#13561=DIRECTION('center_axis',(0.,0.,-1.));
#13562=DIRECTION('ref_axis',(-1.,0.,0.));
#13563=DIRECTION('',(0.,-1.,0.));
#13564=DIRECTION('',(0.,1.,0.));
#13565=DIRECTION('',(1.,0.,0.));
#13566=DIRECTION('center_axis',(0.,-1.,0.));
#13567=DIRECTION('ref_axis',(0.,0.,-1.));
#13568=DIRECTION('center_axis',(0.,-1.,0.));
#13569=DIRECTION('ref_axis',(1.,0.,0.));
#13570=DIRECTION('center_axis',(0.,1.,0.));
#13571=DIRECTION('ref_axis',(1.,0.,0.));
#13572=DIRECTION('',(-1.,0.,0.));
#13573=DIRECTION('center_axis',(0.,0.,1.));
#13574=DIRECTION('ref_axis',(1.,0.,0.));
#13575=DIRECTION('',(0.,1.,0.));
#13576=DIRECTION('',(0.,-1.,0.));
#13577=DIRECTION('center_axis',(0.,1.,0.));
#13578=DIRECTION('ref_axis',(0.,0.,1.));
#13579=DIRECTION('center_axis',(0.,-1.,0.));
#13580=DIRECTION('ref_axis',(1.,0.,0.));
#13581=DIRECTION('center_axis',(0.,-1.,0.));
#13582=DIRECTION('ref_axis',(1.,0.,0.));
#13583=DIRECTION('center_axis',(0.,-1.,0.));
#13584=DIRECTION('ref_axis',(1.,0.,0.));
#13585=DIRECTION('center_axis',(0.,-1.,0.));
#13586=DIRECTION('ref_axis',(1.,0.,0.));
#13587=DIRECTION('',(0.,1.,0.));
#13588=DIRECTION('center_axis',(0.,-1.,0.));
#13589=DIRECTION('ref_axis',(0.,0.,-1.));
#13590=DIRECTION('center_axis',(0.,-1.,0.));
#13591=DIRECTION('ref_axis',(1.,0.,0.));
#13592=DIRECTION('center_axis',(0.,-1.,0.));
#13593=DIRECTION('ref_axis',(1.,0.,0.));
#13594=DIRECTION('',(0.,1.,0.));
#13595=DIRECTION('',(0.,0.,1.));
#13596=DIRECTION('',(1.,0.,0.));
#13597=DIRECTION('',(0.,0.,1.));
#13598=DIRECTION('',(1.,0.,0.));
#13599=DIRECTION('axis',(0.,0.,1.));
#13600=DIRECTION('refdir',(1.,0.,0.));
#13601=DIRECTION('center_axis',(0.,1.,0.));
#13602=DIRECTION('ref_axis',(0.,0.,1.));
#13603=DIRECTION('center_axis',(0.,-1.,0.));
#13604=DIRECTION('ref_axis',(1.,0.,0.));
#13605=DIRECTION('center_axis',(0.,-1.,0.));
#13606=DIRECTION('ref_axis',(1.,0.,0.));
#13607=DIRECTION('center_axis',(0.,-1.,0.));
#13608=DIRECTION('ref_axis',(1.,0.,0.));
#13609=DIRECTION('',(0.707106781186547,0.707106781186548,8.65956056235493E-17));
#13610=DIRECTION('center_axis',(0.,-1.,0.));
#13611=DIRECTION('ref_axis',(1.,0.,0.));
#13612=DIRECTION('center_axis',(0.,-1.,0.));
#13613=DIRECTION('ref_axis',(1.,0.,0.));
#13614=DIRECTION('',(0.,1.,0.));
#13615=DIRECTION('center_axis',(0.,1.,0.));
#13616=DIRECTION('ref_axis',(1.,0.,0.));
#13617=DIRECTION('center_axis',(0.,-1.,0.));
#13618=DIRECTION('ref_axis',(1.,0.,0.));
#13619=DIRECTION('',(-0.707106781186547,0.707106781186548,-8.65956056235493E-17));
#13620=DIRECTION('center_axis',(0.,-1.,0.));
#13621=DIRECTION('ref_axis',(0.,0.,-1.));
#13622=DIRECTION('center_axis',(0.,-1.,0.));
#13623=DIRECTION('ref_axis',(1.,0.,0.));
#13624=DIRECTION('center_axis',(0.,1.,0.));
#13625=DIRECTION('ref_axis',(1.,0.,0.));
#13626=DIRECTION('center_axis',(0.,1.,0.));
#13627=DIRECTION('ref_axis',(1.,0.,0.));
#13628=DIRECTION('',(-0.447213595499958,0.894427190999916,-5.47678698264203E-17));
#13629=DIRECTION('center_axis',(0.,-1.,0.));
#13630=DIRECTION('ref_axis',(1.,0.,0.));
#13631=DIRECTION('center_axis',(0.,1.,0.));
#13632=DIRECTION('ref_axis',(1.,0.,0.));
#13633=DIRECTION('',(0.,1.,0.));
#13634=DIRECTION('center_axis',(0.,1.,0.));
#13635=DIRECTION('ref_axis',(1.,0.,0.));
#13636=DIRECTION('center_axis',(0.,-1.,0.));
#13637=DIRECTION('ref_axis',(1.,0.,0.));
#13638=DIRECTION('',(-0.707106781186547,0.707106781186548,-8.65956056235493E-17));
#13639=DIRECTION('center_axis',(0.,-1.,0.));
#13640=DIRECTION('ref_axis',(0.,0.,-1.));
#13641=DIRECTION('center_axis',(0.866025403784439,0.,-0.5));
#13642=DIRECTION('ref_axis',(0.5,0.,0.866025403784439));
#13643=DIRECTION('',(-0.5,0.,-0.866025403784439));
#13644=DIRECTION('',(0.,-1.,0.));
#13645=DIRECTION('',(0.5,0.,0.866025403784439));
#13646=DIRECTION('',(0.,-1.,0.));
#13647=DIRECTION('center_axis',(1.60246890531964E-16,0.,-1.));
#13648=DIRECTION('ref_axis',(1.,0.,1.60246890531964E-16));
#13649=DIRECTION('',(-1.,0.,-1.60246890531964E-16));
#13650=DIRECTION('',(0.,-1.,0.));
#13651=DIRECTION('',(1.,0.,1.60246890531964E-16));
#13652=DIRECTION('center_axis',(-0.866025403784439,0.,-0.5));
#13653=DIRECTION('ref_axis',(0.5,0.,-0.866025403784439));
#13654=DIRECTION('',(-0.5,0.,0.866025403784439));
#13655=DIRECTION('',(0.,-1.,0.));
#13656=DIRECTION('',(0.5,0.,-0.866025403784439));
#13657=DIRECTION('center_axis',(-0.866025403784439,0.,0.5));
#13658=DIRECTION('ref_axis',(-0.5,0.,-0.866025403784439));
#13659=DIRECTION('',(0.5,0.,0.866025403784439));
#13660=DIRECTION('',(0.,-1.,0.));
#13661=DIRECTION('',(-0.5,0.,-0.866025403784439));
#13662=DIRECTION('center_axis',(-1.60246890531964E-16,0.,1.));
#13663=DIRECTION('ref_axis',(-1.,0.,-1.60246890531964E-16));
#13664=DIRECTION('',(1.,0.,1.60246890531964E-16));
#13665=DIRECTION('',(0.,-1.,0.));
#13666=DIRECTION('',(-1.,0.,-1.60246890531964E-16));
#13667=DIRECTION('center_axis',(0.866025403784439,0.,0.5));
#13668=DIRECTION('ref_axis',(-0.5,0.,0.866025403784439));
#13669=DIRECTION('',(0.5,0.,-0.866025403784439));
#13670=DIRECTION('',(-0.5,0.,0.866025403784439));
#13671=DIRECTION('center_axis',(0.,1.,0.));
#13672=DIRECTION('ref_axis',(1.,0.,0.));
#13673=DIRECTION('center_axis',(0.,-1.,0.));
#13674=DIRECTION('ref_axis',(0.,0.,-1.));
#13675=DIRECTION('',(0.,0.,1.));
#13676=DIRECTION('',(1.,0.,0.));
#13677=DIRECTION('',(0.,0.,1.));
#13678=DIRECTION('',(1.,0.,0.));
#13679=DIRECTION('',(0.,0.,1.));
#13680=DIRECTION('',(1.,0.,0.));
#13681=DIRECTION('',(0.,0.,1.));
#13682=DIRECTION('',(1.,0.,0.));
#13683=DIRECTION('',(0.,0.,1.));
#13684=DIRECTION('',(1.,0.,0.));
#13685=DIRECTION('',(0.,0.,1.));
#13686=DIRECTION('',(1.,0.,0.));
#13687=DIRECTION('',(0.,0.,1.));
#13688=DIRECTION('',(1.,0.,0.));
#13689=DIRECTION('',(0.,0.,1.));
#13690=DIRECTION('',(1.,0.,0.));
#13691=DIRECTION('',(0.,0.,1.));
#13692=DIRECTION('',(1.,0.,0.));
#13693=DIRECTION('',(0.,0.,1.));
#13694=DIRECTION('',(1.,0.,0.));
#13695=DIRECTION('',(0.,0.,1.));
#13696=DIRECTION('',(1.,0.,0.));
#13697=DIRECTION('',(0.,0.,1.));
#13698=DIRECTION('',(1.,0.,0.));
#13699=DIRECTION('',(0.,0.,1.));
#13700=DIRECTION('',(1.,0.,0.));
#13701=DIRECTION('',(0.,0.,1.));
#13702=DIRECTION('',(1.,0.,0.));
#13703=DIRECTION('',(0.,0.,1.));
#13704=DIRECTION('',(1.,0.,0.));
#13705=DIRECTION('',(0.,0.,1.));
#13706=DIRECTION('',(1.,0.,0.));
#13707=DIRECTION('',(0.,0.,1.));
#13708=DIRECTION('',(1.,0.,0.));
#13709=DIRECTION('',(0.,0.,1.));
#13710=DIRECTION('',(1.,0.,0.));
#13711=DIRECTION('',(0.,0.,1.));
#13712=DIRECTION('',(1.,0.,0.));
#13713=DIRECTION('',(0.,0.,1.));
#13714=DIRECTION('',(1.,0.,0.));
#13715=DIRECTION('',(0.,0.,1.));
#13716=DIRECTION('',(1.,0.,0.));
#13717=DIRECTION('',(0.,0.,1.));
#13718=DIRECTION('',(1.,0.,0.));
#13719=DIRECTION('',(0.,0.,1.));
#13720=DIRECTION('',(1.,0.,0.));
#13721=DIRECTION('',(0.,0.,1.));
#13722=DIRECTION('',(1.,0.,0.));
#13723=DIRECTION('',(0.,0.,1.));
#13724=DIRECTION('',(1.,0.,0.));
#13725=DIRECTION('',(0.,0.,1.));
#13726=DIRECTION('',(1.,0.,0.));
#13727=DIRECTION('',(0.,0.,1.));
#13728=DIRECTION('',(1.,0.,0.));
#13729=DIRECTION('',(0.,0.,1.));
#13730=DIRECTION('',(1.,0.,0.));
#13731=DIRECTION('',(0.,0.,1.));
#13732=DIRECTION('',(1.,0.,0.));
#13733=DIRECTION('',(0.,0.,1.));
#13734=DIRECTION('',(1.,0.,0.));
#13735=DIRECTION('',(0.,0.,1.));
#13736=DIRECTION('',(1.,0.,0.));
#13737=DIRECTION('',(0.,0.,1.));
#13738=DIRECTION('',(1.,0.,0.));
#13739=DIRECTION('',(0.,0.,1.));
#13740=DIRECTION('',(1.,0.,0.));
#13741=DIRECTION('',(0.,1.,2.22044604925031E-16));
#13742=DIRECTION('',(1.,0.,0.));
#13743=DIRECTION('',(0.,-1.,2.22044604925031E-16));
#13744=DIRECTION('',(1.,0.,0.));
#13745=DIRECTION('',(0.,1.,2.22044604925031E-16));
#13746=DIRECTION('',(1.,0.,0.));
#13747=DIRECTION('',(0.,-1.,2.22044604925031E-16));
#13748=DIRECTION('',(1.,0.,0.));
#13749=DIRECTION('',(0.,1.,2.22044604925031E-16));
#13750=DIRECTION('',(1.,0.,0.));
#13751=DIRECTION('',(0.,-1.,2.22044604925031E-16));
#13752=DIRECTION('',(1.,0.,0.));
#13753=DIRECTION('',(0.,1.,2.22044604925031E-16));
#13754=DIRECTION('',(1.,0.,0.));
#13755=DIRECTION('',(0.,-1.,2.22044604925031E-16));
#13756=DIRECTION('',(1.,0.,0.));
#13757=DIRECTION('',(-1.,0.,2.22044604925031E-16));
#13758=DIRECTION('',(2.22044604925031E-16,0.,1.));
#13759=DIRECTION('',(0.,-1.,2.22044604925031E-16));
#13760=DIRECTION('',(1.,0.,0.));
#13761=DIRECTION('',(0.,0.,1.));
#13762=DIRECTION('',(-1.,1.22464679914735E-16,0.));
#13763=DIRECTION('',(0.,0.,1.));
#13764=DIRECTION('',(-1.,1.22464679914735E-16,0.));
#13765=DIRECTION('',(0.,0.,1.));
#13766=DIRECTION('',(2.22044604925031E-16,-1.,0.));
#13767=DIRECTION('',(0.,1.,2.22044604925031E-16));
#13768=DIRECTION('',(1.,0.,0.));
#13769=DIRECTION('',(0.,1.,2.22044604925031E-16));
#13770=DIRECTION('',(1.,0.,0.));
#13771=DIRECTION('',(0.,-1.,2.22044604925031E-16));
#13772=DIRECTION('',(1.,0.,0.));
#13773=DIRECTION('',(0.,0.,1.));
#13774=DIRECTION('',(-1.,1.22464679914735E-16,0.));
#13775=DIRECTION('',(0.,0.,1.));
#13776=DIRECTION('',(-1.,1.22464679914735E-16,0.));
#13777=DIRECTION('',(0.,0.,1.));
#13778=DIRECTION('',(2.22044604925031E-16,-1.,0.));
#13779=DIRECTION('',(0.,-1.,2.22044604925031E-16));
#13780=DIRECTION('',(1.,0.,0.));
#13781=DIRECTION('',(0.,-1.,2.22044604925031E-16));
#13782=DIRECTION('',(1.,0.,0.));
#13783=DIRECTION('',(-1.,0.,2.22044604925031E-16));
#13784=DIRECTION('',(2.22044604925031E-16,0.,1.));
#13785=DIRECTION('',(0.,-1.,2.22044604925031E-16));
#13786=DIRECTION('',(1.,0.,0.));
#13787=DIRECTION('',(0.,0.,1.));
#13788=DIRECTION('',(-1.,1.22464679914735E-16,0.));
#13789=DIRECTION('',(0.,0.,1.));
#13790=DIRECTION('',(-1.,1.22464679914735E-16,0.));
#13791=DIRECTION('',(0.,0.,1.));
#13792=DIRECTION('',(2.22044604925031E-16,-1.,0.));
#13793=DIRECTION('',(0.,1.,2.22044604925031E-16));
#13794=DIRECTION('',(1.,0.,0.));
#13795=DIRECTION('',(0.,1.,2.22044604925031E-16));
#13796=DIRECTION('',(1.,0.,0.));
#13797=DIRECTION('',(0.,-1.,2.22044604925031E-16));
#13798=DIRECTION('',(1.,0.,0.));
#13799=DIRECTION('',(0.,0.,1.));
#13800=DIRECTION('',(-1.,1.22464679914735E-16,0.));
#13801=DIRECTION('',(0.,0.,1.));
#13802=DIRECTION('',(-1.,1.22464679914735E-16,0.));
#13803=DIRECTION('',(0.,0.,1.));
#13804=DIRECTION('',(2.22044604925031E-16,-1.,0.));
#13805=DIRECTION('',(0.,-1.,2.22044604925031E-16));
#13806=DIRECTION('',(1.,0.,0.));
#13807=DIRECTION('',(0.,-1.,2.22044604925031E-16));
#13808=DIRECTION('',(1.,0.,0.));
#13809=DIRECTION('',(-1.,0.,2.22044604925031E-16));
#13810=DIRECTION('',(2.22044604925031E-16,0.,1.));
#13811=DIRECTION('',(0.,-1.,2.22044604925031E-16));
#13812=DIRECTION('',(1.,0.,0.));
#13813=DIRECTION('',(0.,0.,1.));
#13814=DIRECTION('',(-1.,1.22464679914735E-16,0.));
#13815=DIRECTION('',(0.,0.,1.));
#13816=DIRECTION('',(-1.,1.22464679914735E-16,0.));
#13817=DIRECTION('',(0.,0.,1.));
#13818=DIRECTION('',(2.22044604925031E-16,-1.,0.));
#13819=DIRECTION('',(0.,1.,2.22044604925031E-16));
#13820=DIRECTION('',(1.,0.,0.));
#13821=DIRECTION('',(0.,1.,2.22044604925031E-16));
#13822=DIRECTION('',(1.,0.,0.));
#13823=DIRECTION('',(0.,-1.,2.22044604925031E-16));
#13824=DIRECTION('',(1.,0.,0.));
#13825=DIRECTION('',(0.,0.,1.));
#13826=DIRECTION('',(-1.,1.22464679914735E-16,0.));
#13827=DIRECTION('',(0.,0.,1.));
#13828=DIRECTION('',(-1.,1.22464679914735E-16,0.));
#13829=DIRECTION('',(0.,0.,1.));
#13830=DIRECTION('',(2.22044604925031E-16,-1.,0.));
#13831=DIRECTION('',(0.,-1.,2.22044604925031E-16));
#13832=DIRECTION('',(1.,0.,0.));
#13833=DIRECTION('',(0.,-1.,2.22044604925031E-16));
#13834=DIRECTION('',(1.,0.,0.));
#13835=DIRECTION('',(-1.,0.,2.22044604925031E-16));
#13836=DIRECTION('',(2.22044604925031E-16,0.,1.));
#13837=DIRECTION('',(0.,-1.,2.22044604925031E-16));
#13838=DIRECTION('',(1.,0.,0.));
#13839=DIRECTION('',(0.,0.,1.));
#13840=DIRECTION('',(-1.,1.22464679914735E-16,0.));
#13841=DIRECTION('',(0.,0.,1.));
#13842=DIRECTION('',(-1.,1.22464679914735E-16,0.));
#13843=DIRECTION('',(0.,0.,1.));
#13844=DIRECTION('',(2.22044604925031E-16,-1.,0.));
#13845=DIRECTION('',(0.,1.,2.22044604925031E-16));
#13846=DIRECTION('',(1.,0.,0.));
#13847=DIRECTION('',(0.,1.,2.22044604925031E-16));
#13848=DIRECTION('',(1.,0.,0.));
#13849=DIRECTION('',(0.,-1.,2.22044604925031E-16));
#13850=DIRECTION('',(1.,0.,0.));
#13851=DIRECTION('',(0.,0.,1.));
#13852=DIRECTION('',(-1.,1.22464679914735E-16,0.));
#13853=DIRECTION('',(0.,0.,1.));
#13854=DIRECTION('',(-1.,1.22464679914735E-16,0.));
#13855=DIRECTION('',(0.,0.,1.));
#13856=DIRECTION('',(2.22044604925031E-16,-1.,0.));
#13857=DIRECTION('',(0.,-1.,2.22044604925031E-16));
#13858=DIRECTION('',(1.,0.,0.));
#13859=DIRECTION('',(0.,-1.,2.22044604925031E-16));
#13860=DIRECTION('',(1.,0.,0.));
#13861=DIRECTION('',(0.,-1.,2.22044604925031E-16));
#13862=DIRECTION('',(1.,0.,0.));
#13863=DIRECTION('',(0.,-1.,2.22044604925031E-16));
#13864=DIRECTION('',(1.,0.,0.));
#13865=DIRECTION('',(0.,-1.,2.22044604925031E-16));
#13866=DIRECTION('',(1.,0.,0.));
#13867=DIRECTION('',(0.,-1.,2.22044604925031E-16));
#13868=DIRECTION('',(1.,0.,0.));
#13869=DIRECTION('',(0.,1.,2.22044604925031E-16));
#13870=DIRECTION('',(1.,0.,0.));
#13871=DIRECTION('',(0.,1.,2.22044604925031E-16));
#13872=DIRECTION('',(1.,0.,0.));
#13873=DIRECTION('',(0.,1.,2.22044604925031E-16));
#13874=DIRECTION('',(1.,0.,0.));
#13875=DIRECTION('',(0.,1.,2.22044604925031E-16));
#13876=DIRECTION('',(1.,0.,0.));
#13877=DIRECTION('',(0.,1.,2.22044604925031E-16));
#13878=DIRECTION('',(1.,0.,0.));
#13879=DIRECTION('',(0.,-1.,2.22044604925031E-16));
#13880=DIRECTION('',(1.,0.,0.));
#13881=DIRECTION('',(0.,1.,2.22044604925031E-16));
#13882=DIRECTION('',(1.,0.,0.));
#13883=DIRECTION('',(0.,-1.,2.22044604925031E-16));
#13884=DIRECTION('',(1.,0.,0.));
#13885=DIRECTION('',(0.,0.,1.));
#13886=DIRECTION('',(1.,0.,0.));
#13887=DIRECTION('',(0.,0.,1.));
#13888=DIRECTION('',(1.,0.,0.));
#13889=DIRECTION('',(0.,0.,1.));
#13890=DIRECTION('',(1.,0.,0.));
#13891=DIRECTION('',(0.,0.,1.));
#13892=DIRECTION('',(1.,0.,0.));
#13893=DIRECTION('',(0.,0.,1.));
#13894=DIRECTION('',(1.,0.,0.));
#13895=DIRECTION('',(0.,0.,1.));
#13896=DIRECTION('',(1.,0.,0.));
#13897=DIRECTION('',(0.,-1.,2.22044604925031E-16));
#13898=DIRECTION('',(1.,0.,0.));
#13899=DIRECTION('',(0.,-1.,2.22044604925031E-16));
#13900=DIRECTION('',(1.,0.,0.));
#13901=DIRECTION('',(0.,-1.,2.22044604925031E-16));
#13902=DIRECTION('',(1.,0.,0.));
#13903=DIRECTION('',(0.,-1.,2.22044604925031E-16));
#13904=DIRECTION('',(1.,0.,0.));
#13905=DIRECTION('',(0.,-1.,2.22044604925031E-16));
#13906=DIRECTION('',(1.,0.,0.));
#13907=DIRECTION('',(0.,-1.,2.22044604925031E-16));
#13908=DIRECTION('',(1.,0.,0.));
#13909=DIRECTION('',(0.,-1.,2.22044604925031E-16));
#13910=DIRECTION('',(1.,0.,0.));
#13911=DIRECTION('',(0.,-1.,2.22044604925031E-16));
#13912=DIRECTION('',(1.,0.,0.));
#13913=DIRECTION('',(0.,-1.,2.22044604925031E-16));
#13914=DIRECTION('',(1.,0.,0.));
#13915=DIRECTION('',(0.,-1.,2.22044604925031E-16));
#13916=DIRECTION('',(1.,0.,0.));
#13917=DIRECTION('',(0.,-1.,2.22044604925031E-16));
#13918=DIRECTION('',(1.,0.,0.));
#13919=DIRECTION('',(0.,-1.,2.22044604925031E-16));
#13920=DIRECTION('',(1.,0.,0.));
#13921=DIRECTION('',(0.,-1.,2.22044604925031E-16));
#13922=DIRECTION('',(1.,0.,0.));
#13923=DIRECTION('',(0.,-1.,2.22044604925031E-16));
#13924=DIRECTION('',(1.,0.,0.));
#13925=DIRECTION('',(0.,-1.,2.22044604925031E-16));
#13926=DIRECTION('',(1.,0.,0.));
#13927=DIRECTION('',(0.,-1.,2.22044604925031E-16));
#13928=DIRECTION('',(1.,0.,0.));
#13929=DIRECTION('',(0.,-1.,2.22044604925031E-16));
#13930=DIRECTION('',(1.,0.,0.));
#13931=DIRECTION('',(0.,-1.,2.22044604925031E-16));
#13932=DIRECTION('',(1.,0.,0.));
#13933=DIRECTION('',(0.,-1.,2.22044604925031E-16));
#13934=DIRECTION('',(1.,0.,0.));
#13935=DIRECTION('',(0.,-1.,2.22044604925031E-16));
#13936=DIRECTION('',(1.,0.,0.));
#13937=DIRECTION('',(0.,-1.,2.22044604925031E-16));
#13938=DIRECTION('',(1.,0.,0.));
#13939=DIRECTION('',(0.,-1.,2.22044604925031E-16));
#13940=DIRECTION('',(1.,0.,0.));
#13941=DIRECTION('',(0.,-1.,2.22044604925031E-16));
#13942=DIRECTION('',(1.,0.,0.));
#13943=DIRECTION('',(0.,-1.,2.22044604925031E-16));
#13944=DIRECTION('',(1.,0.,0.));
#13945=DIRECTION('',(0.,0.,1.));
#13946=DIRECTION('',(1.,0.,0.));
#13947=DIRECTION('',(0.,0.,1.));
#13948=DIRECTION('',(1.,0.,0.));
#13949=CARTESIAN_POINT('',(0.,0.,0.));
#13950=CARTESIAN_POINT('',(0.,0.,0.));
#13951=CARTESIAN_POINT('',(0.,0.,0.));
#13952=CARTESIAN_POINT('Origin',(0.,6.,-1.3));
#13953=CARTESIAN_POINT('',(-0.275,6.,-1.2));
#13954=CARTESIAN_POINT('Origin',(0.,6.,-1.2));
#13955=CARTESIAN_POINT('',(-0.275,6.,0.));
#13956=CARTESIAN_POINT('',(-0.275,6.,-1.3));
#13957=CARTESIAN_POINT('Origin',(0.,6.,0.));
#13958=CARTESIAN_POINT('Origin',(0.,-6.,-1.3));
#13959=CARTESIAN_POINT('',(-0.275,-6.,-1.2));
#13960=CARTESIAN_POINT('Origin',(0.,-6.,-1.2));
#13961=CARTESIAN_POINT('',(-0.275,-6.,0.));
#13962=CARTESIAN_POINT('',(-0.275,-6.,-1.3));
#13963=CARTESIAN_POINT('Origin',(0.,-6.,0.));
#13964=CARTESIAN_POINT('Origin',(1.8,-1.8,-1.3));
#13965=CARTESIAN_POINT('',(1.3,-1.8,-1.2));
#13966=CARTESIAN_POINT('Origin',(1.8,-1.8,-1.2));
#13967=CARTESIAN_POINT('',(1.3,-1.8,0.));
#13968=CARTESIAN_POINT('',(1.3,-1.8,-1.3));
#13969=CARTESIAN_POINT('Origin',(1.8,-1.8,0.));
#13970=CARTESIAN_POINT('Origin',(-1.8,1.8,-1.3));
#13971=CARTESIAN_POINT('',(-2.3,1.8,-1.2));
#13972=CARTESIAN_POINT('Origin',(-1.8,1.8,-1.2));
#13973=CARTESIAN_POINT('',(-2.3,1.8,0.));
#13974=CARTESIAN_POINT('',(-2.3,1.8,-1.3));
#13975=CARTESIAN_POINT('Origin',(-1.8,1.8,0.));
#13976=CARTESIAN_POINT('Origin',(-1.8,-1.8,-1.3));
#13977=CARTESIAN_POINT('',(-2.3,-1.8,-1.2));
#13978=CARTESIAN_POINT('Origin',(-1.8,-1.8,-1.2));
#13979=CARTESIAN_POINT('',(-2.3,-1.8,0.));
#13980=CARTESIAN_POINT('',(-2.3,-1.8,-1.3));
#13981=CARTESIAN_POINT('Origin',(-1.8,-1.8,0.));
#13982=CARTESIAN_POINT('Origin',(1.8,1.8,-1.3));
#13983=CARTESIAN_POINT('',(1.3,1.8,-1.2));
#13984=CARTESIAN_POINT('Origin',(1.8,1.8,-1.2));
#13985=CARTESIAN_POINT('',(1.3,1.8,0.));
#13986=CARTESIAN_POINT('',(1.3,1.8,-1.3));
#13987=CARTESIAN_POINT('Origin',(1.8,1.8,0.));
#13988=CARTESIAN_POINT('Origin',(2.9,-2.9,-1.3));
#13989=CARTESIAN_POINT('',(2.69,-2.9,-1.2));
#13990=CARTESIAN_POINT('Origin',(2.9,-2.9,-1.2));
#13991=CARTESIAN_POINT('',(2.69,-2.9,0.));
#13992=CARTESIAN_POINT('',(2.69,-2.9,-1.3));
#13993=CARTESIAN_POINT('Origin',(2.9,-2.9,0.));
#13994=CARTESIAN_POINT('Origin',(-2.9,2.9,-1.3));
#13995=CARTESIAN_POINT('',(-3.11,2.9,-1.2));
#13996=CARTESIAN_POINT('Origin',(-2.9,2.9,-1.2));
#13997=CARTESIAN_POINT('',(-3.11,2.9,0.));
#13998=CARTESIAN_POINT('',(-3.11,2.9,-1.3));
#13999=CARTESIAN_POINT('Origin',(-2.9,2.9,0.));
#14000=CARTESIAN_POINT('Origin',(-2.9,-2.9,-1.3));
#14001=CARTESIAN_POINT('',(-3.11,-2.9,-1.2));
#14002=CARTESIAN_POINT('Origin',(-2.9,-2.9,-1.2));
#14003=CARTESIAN_POINT('',(-3.11,-2.9,0.));
#14004=CARTESIAN_POINT('',(-3.11,-2.9,-1.3));
#14005=CARTESIAN_POINT('Origin',(-2.9,-2.9,0.));
#14006=CARTESIAN_POINT('Origin',(2.9,2.9,-1.3));
#14007=CARTESIAN_POINT('',(2.69,2.9,-1.2));
#14008=CARTESIAN_POINT('Origin',(2.9,2.9,-1.2));
#14009=CARTESIAN_POINT('',(2.69,2.9,0.));
#14010=CARTESIAN_POINT('',(2.69,2.9,-1.3));
#14011=CARTESIAN_POINT('Origin',(2.9,2.9,0.));
#14012=CARTESIAN_POINT('Origin',(4.4,6.7,-1.3));
#14013=CARTESIAN_POINT('',(4.125,6.7,-1.2));
#14014=CARTESIAN_POINT('Origin',(4.4,6.7,-1.2));
#14015=CARTESIAN_POINT('',(4.125,6.7,0.));
#14016=CARTESIAN_POINT('',(4.125,6.7,-1.3));
#14017=CARTESIAN_POINT('Origin',(4.4,6.7,0.));
#14018=CARTESIAN_POINT('Origin',(7.6,6.7,-1.3));
#14019=CARTESIAN_POINT('',(7.325,6.7,-1.2));
#14020=CARTESIAN_POINT('Origin',(7.6,6.7,-1.2));
#14021=CARTESIAN_POINT('',(7.325,6.7,0.));
#14022=CARTESIAN_POINT('',(7.325,6.7,-1.3));
#14023=CARTESIAN_POINT('Origin',(7.6,6.7,0.));
#14024=CARTESIAN_POINT('Origin',(4.4,-1.3,-1.3));
#14025=CARTESIAN_POINT('',(4.125,-1.3,-1.2));
#14026=CARTESIAN_POINT('Origin',(4.4,-1.3,-1.2));
#14027=CARTESIAN_POINT('',(4.125,-1.3,0.));
#14028=CARTESIAN_POINT('',(4.125,-1.3,-1.3));
#14029=CARTESIAN_POINT('Origin',(4.4,-1.3,0.));
#14030=CARTESIAN_POINT('Origin',(7.6,-1.3,-1.3));
#14031=CARTESIAN_POINT('',(7.325,-1.3,-1.2));
#14032=CARTESIAN_POINT('Origin',(7.6,-1.3,-1.2));
#14033=CARTESIAN_POINT('',(7.325,-1.3,0.));
#14034=CARTESIAN_POINT('',(7.325,-1.3,-1.3));
#14035=CARTESIAN_POINT('Origin',(7.6,-1.3,0.));
#14036=CARTESIAN_POINT('Origin',(-7.6,6.7,-1.3));
#14037=CARTESIAN_POINT('',(-7.875,6.7,-1.2));
#14038=CARTESIAN_POINT('Origin',(-7.6,6.7,-1.2));
#14039=CARTESIAN_POINT('',(-7.875,6.7,0.));
#14040=CARTESIAN_POINT('',(-7.875,6.7,-1.3));
#14041=CARTESIAN_POINT('Origin',(-7.6,6.7,0.));
#14042=CARTESIAN_POINT('Origin',(-4.4,6.7,-1.3));
#14043=CARTESIAN_POINT('',(-4.675,6.7,-1.2));
#14044=CARTESIAN_POINT('Origin',(-4.4,6.7,-1.2));
#14045=CARTESIAN_POINT('',(-4.675,6.7,0.));
#14046=CARTESIAN_POINT('',(-4.675,6.7,-1.3));
#14047=CARTESIAN_POINT('Origin',(-4.4,6.7,0.));
#14048=CARTESIAN_POINT('Origin',(-7.6,-1.3,-1.3));
#14049=CARTESIAN_POINT('',(-7.875,-1.3,-1.2));
#14050=CARTESIAN_POINT('Origin',(-7.6,-1.3,-1.2));
#14051=CARTESIAN_POINT('',(-7.875,-1.3,0.));
#14052=CARTESIAN_POINT('',(-7.875,-1.3,-1.3));
#14053=CARTESIAN_POINT('Origin',(-7.6,-1.3,0.));
#14054=CARTESIAN_POINT('Origin',(-4.4,-1.3,-1.3));
#14055=CARTESIAN_POINT('',(-4.675,-1.3,-1.2));
#14056=CARTESIAN_POINT('Origin',(-4.4,-1.3,-1.2));
#14057=CARTESIAN_POINT('',(-4.675,-1.3,0.));
#14058=CARTESIAN_POINT('',(-4.675,-1.3,-1.3));
#14059=CARTESIAN_POINT('Origin',(-4.4,-1.3,0.));
#14060=CARTESIAN_POINT('Origin',(9.5,10.,-1.3));
#14061=CARTESIAN_POINT('',(9.225,10.,-1.2));
#14062=CARTESIAN_POINT('Origin',(9.5,10.,-1.2));
#14063=CARTESIAN_POINT('',(9.225,10.,0.));
#14064=CARTESIAN_POINT('',(9.225,10.,-1.3));
#14065=CARTESIAN_POINT('Origin',(9.5,10.,0.));
#14066=CARTESIAN_POINT('Origin',(9.5,11.,-1.3));
#14067=CARTESIAN_POINT('',(9.225,11.,-1.2));
#14068=CARTESIAN_POINT('Origin',(9.5,11.,-1.2));
#14069=CARTESIAN_POINT('',(9.225,11.,0.));
#14070=CARTESIAN_POINT('',(9.225,11.,-1.3));
#14071=CARTESIAN_POINT('Origin',(9.5,11.,0.));
#14072=CARTESIAN_POINT('Origin',(-9.5,10.,-1.3));
#14073=CARTESIAN_POINT('',(-9.775,10.,-1.2));
#14074=CARTESIAN_POINT('Origin',(-9.5,10.,-1.2));
#14075=CARTESIAN_POINT('',(-9.775,10.,0.));
#14076=CARTESIAN_POINT('',(-9.775,10.,-1.3));
#14077=CARTESIAN_POINT('Origin',(-9.5,10.,0.));
#14078=CARTESIAN_POINT('Origin',(-9.5,11.,-1.3));
#14079=CARTESIAN_POINT('',(-9.775,11.,-1.2));
#14080=CARTESIAN_POINT('Origin',(-9.5,11.,-1.2));
#14081=CARTESIAN_POINT('',(-9.775,11.,0.));
#14082=CARTESIAN_POINT('',(-9.775,11.,-1.3));
#14083=CARTESIAN_POINT('Origin',(-9.5,11.,0.));
#14084=CARTESIAN_POINT('Origin',(11.,12.5,-1.2));
#14085=CARTESIAN_POINT('',(11.,12.5,-1.2));
#14086=CARTESIAN_POINT('',(-11.,12.5,-1.2));
#14087=CARTESIAN_POINT('',(11.,12.5,-1.2));
#14088=CARTESIAN_POINT('',(-11.,12.5,0.));
#14089=CARTESIAN_POINT('',(-11.,12.5,-1.2));
#14090=CARTESIAN_POINT('',(11.,12.5,0.));
#14091=CARTESIAN_POINT('',(11.,12.5,0.));
#14092=CARTESIAN_POINT('',(11.,12.5,-1.2));
#14093=CARTESIAN_POINT('Origin',(11.,-8.,-1.2));
#14094=CARTESIAN_POINT('',(11.,-8.,-1.2));
#14095=CARTESIAN_POINT('',(11.,-8.,-1.2));
#14096=CARTESIAN_POINT('',(11.,-8.,0.));
#14097=CARTESIAN_POINT('',(11.,-8.,0.));
#14098=CARTESIAN_POINT('',(11.,-8.,-1.2));
#14099=CARTESIAN_POINT('Origin',(-11.,-8.,-1.2));
#14100=CARTESIAN_POINT('',(-11.,-8.,-1.2));
#14101=CARTESIAN_POINT('',(-11.,-8.,-1.2));
#14102=CARTESIAN_POINT('',(-11.,-8.,0.));
#14103=CARTESIAN_POINT('',(-11.,-8.,0.));
#14104=CARTESIAN_POINT('',(-11.,-8.,-1.2));
#14105=CARTESIAN_POINT('Origin',(-11.,12.5,-1.2));
#14106=CARTESIAN_POINT('',(-11.,12.5,-1.2));
#14107=CARTESIAN_POINT('',(-11.,12.5,0.));
#14108=CARTESIAN_POINT('Origin',(0.,2.25,0.));
#14109=CARTESIAN_POINT('Origin',(0.,2.25,-1.2));
#14110=CARTESIAN_POINT('',(0.,0.,0.));
#14111=CARTESIAN_POINT('Origin',(11.,-7.2,-2.2));
#14112=CARTESIAN_POINT('',(11.,-7.2,-2.2));
#14113=CARTESIAN_POINT('',(-11.,-7.2,-2.2));
#14114=CARTESIAN_POINT('',(11.,-7.2,-2.2));
#14115=CARTESIAN_POINT('',(-11.,-7.2,-1.2));
#14116=CARTESIAN_POINT('',(-11.,-7.2,-2.2));
#14117=CARTESIAN_POINT('',(11.,-7.2,-1.2));
#14118=CARTESIAN_POINT('',(11.,-7.2,-1.2));
#14119=CARTESIAN_POINT('',(11.,-7.2,-2.2));
#14120=CARTESIAN_POINT('Origin',(11.,-8.,-2.2));
#14121=CARTESIAN_POINT('',(11.,-8.,-2.2));
#14122=CARTESIAN_POINT('',(11.,-8.,-2.2));
#14123=CARTESIAN_POINT('',(11.,-8.,-1.2));
#14124=CARTESIAN_POINT('',(11.,-8.,-1.2));
#14125=CARTESIAN_POINT('',(11.,-8.,-2.2));
#14126=CARTESIAN_POINT('Origin',(-11.,-8.,-2.2));
#14127=CARTESIAN_POINT('',(-11.,-8.,-2.2));
#14128=CARTESIAN_POINT('',(-11.,-8.,-2.2));
#14129=CARTESIAN_POINT('',(-11.,-8.,-1.2));
#14130=CARTESIAN_POINT('',(-11.,-8.,-1.2));
#14131=CARTESIAN_POINT('',(-11.,-8.,-2.2));
#14132=CARTESIAN_POINT('Origin',(-11.,-7.2,-2.2));
#14133=CARTESIAN_POINT('',(-11.,-7.2,-2.2));
#14134=CARTESIAN_POINT('',(-11.,-7.2,-1.2));
#14135=CARTESIAN_POINT('Origin',(0.,-7.6,-1.2));
#14136=CARTESIAN_POINT('Origin',(0.,-7.6,-2.2));
#14137=CARTESIAN_POINT('',(0.,0.,0.));
#14138=CARTESIAN_POINT('Origin',(11.,12.5,-2.2));
#14139=CARTESIAN_POINT('',(11.,12.5,-2.2));
#14140=CARTESIAN_POINT('',(-11.,12.5,-2.2));
#14141=CARTESIAN_POINT('',(11.,12.5,-2.2));
#14142=CARTESIAN_POINT('',(-11.,12.5,-1.2));
#14143=CARTESIAN_POINT('',(-11.,12.5,-2.2));
#14144=CARTESIAN_POINT('',(11.,12.5,-1.2));
#14145=CARTESIAN_POINT('',(11.,12.5,-1.2));
#14146=CARTESIAN_POINT('',(11.,12.5,-2.2));
#14147=CARTESIAN_POINT('Origin',(11.,11.7,-2.2));
#14148=CARTESIAN_POINT('',(11.,11.7,-2.2));
#14149=CARTESIAN_POINT('',(11.,11.7,-2.2));
#14150=CARTESIAN_POINT('',(11.,11.7,-1.2));
#14151=CARTESIAN_POINT('',(11.,11.7,-1.2));
#14152=CARTESIAN_POINT('',(11.,11.7,-2.2));
#14153=CARTESIAN_POINT('Origin',(-11.,11.7,-2.2));
#14154=CARTESIAN_POINT('',(-11.,11.7,-2.2));
#14155=CARTESIAN_POINT('',(-11.,11.7,-2.2));
#14156=CARTESIAN_POINT('',(-11.,11.7,-1.2));
#14157=CARTESIAN_POINT('',(-11.,11.7,-1.2));
#14158=CARTESIAN_POINT('',(-11.,11.7,-2.2));
#14159=CARTESIAN_POINT('Origin',(-11.,12.5,-2.2));
#14160=CARTESIAN_POINT('',(-11.,12.5,-2.2));
#14161=CARTESIAN_POINT('',(-11.,12.5,-1.2));
#14162=CARTESIAN_POINT('Origin',(0.,12.1,-1.2));
#14163=CARTESIAN_POINT('Origin',(0.,12.1,-2.2));
#14164=CARTESIAN_POINT('',(0.,0.,0.));
#14165=CARTESIAN_POINT('Origin',(0.,6.,30.4));
#14166=CARTESIAN_POINT('',(-0.275,6.,30.5));
#14167=CARTESIAN_POINT('Origin',(0.,6.,30.5));
#14168=CARTESIAN_POINT('',(-0.275,6.,31.5));
#14169=CARTESIAN_POINT('',(-0.275,6.,30.4));
#14170=CARTESIAN_POINT('Origin',(0.,6.,31.5));
#14171=CARTESIAN_POINT('Origin',(0.,-6.,30.4));
#14172=CARTESIAN_POINT('',(-0.275,-6.,30.5));
#14173=CARTESIAN_POINT('Origin',(0.,-6.,30.5));
#14174=CARTESIAN_POINT('',(-0.275,-6.,31.5));
#14175=CARTESIAN_POINT('',(-0.275,-6.,30.4));
#14176=CARTESIAN_POINT('Origin',(0.,-6.,31.5));
#14177=CARTESIAN_POINT('Origin',(4.4,8.,30.4));
#14178=CARTESIAN_POINT('',(4.125,8.,30.5));
#14179=CARTESIAN_POINT('Origin',(4.4,8.,30.5));
#14180=CARTESIAN_POINT('',(4.125,8.,31.5));
#14181=CARTESIAN_POINT('',(4.125,8.,30.4));
#14182=CARTESIAN_POINT('Origin',(4.4,8.,31.5));
#14183=CARTESIAN_POINT('Origin',(7.6,8.,30.4));
#14184=CARTESIAN_POINT('',(7.325,8.,30.5));
#14185=CARTESIAN_POINT('Origin',(7.6,8.,30.5));
#14186=CARTESIAN_POINT('',(7.325,8.,31.5));
#14187=CARTESIAN_POINT('',(7.325,8.,30.4));
#14188=CARTESIAN_POINT('Origin',(7.6,8.,31.5));
#14189=CARTESIAN_POINT('Origin',(4.4,0.,30.4));
#14190=CARTESIAN_POINT('',(4.125,-3.36777869765523E-17,30.5));
#14191=CARTESIAN_POINT('Origin',(4.4,0.,30.5));
#14192=CARTESIAN_POINT('',(4.125,3.36777869765523E-17,31.5));
#14193=CARTESIAN_POINT('',(4.125,-3.36777869765523E-17,30.4));
#14194=CARTESIAN_POINT('Origin',(4.4,0.,31.5));
#14195=CARTESIAN_POINT('Origin',(7.6,0.,30.4));
#14196=CARTESIAN_POINT('',(7.325,-3.36777869765523E-17,30.5));
#14197=CARTESIAN_POINT('Origin',(7.6,0.,30.5));
#14198=CARTESIAN_POINT('',(7.325,3.36777869765523E-17,31.5));
#14199=CARTESIAN_POINT('',(7.325,-3.36777869765523E-17,30.4));
#14200=CARTESIAN_POINT('Origin',(7.6,0.,31.5));
#14201=CARTESIAN_POINT('Origin',(-7.6,8.,30.4));
#14202=CARTESIAN_POINT('',(-7.875,8.,30.5));
#14203=CARTESIAN_POINT('Origin',(-7.6,8.,30.5));
#14204=CARTESIAN_POINT('',(-7.875,8.,31.5));
#14205=CARTESIAN_POINT('',(-7.875,8.,30.4));
#14206=CARTESIAN_POINT('Origin',(-7.6,8.,31.5));
#14207=CARTESIAN_POINT('Origin',(-4.4,8.,30.4));
#14208=CARTESIAN_POINT('',(-4.675,8.,30.5));
#14209=CARTESIAN_POINT('Origin',(-4.4,8.,30.5));
#14210=CARTESIAN_POINT('',(-4.675,8.,31.5));
#14211=CARTESIAN_POINT('',(-4.675,8.,30.4));
#14212=CARTESIAN_POINT('Origin',(-4.4,8.,31.5));
#14213=CARTESIAN_POINT('Origin',(-7.6,0.,30.4));
#14214=CARTESIAN_POINT('',(-7.875,-3.36777869765523E-17,30.5));
#14215=CARTESIAN_POINT('Origin',(-7.6,0.,30.5));
#14216=CARTESIAN_POINT('',(-7.875,3.36777869765523E-17,31.5));
#14217=CARTESIAN_POINT('',(-7.875,-3.36777869765523E-17,30.4));
#14218=CARTESIAN_POINT('Origin',(-7.6,0.,31.5));
#14219=CARTESIAN_POINT('Origin',(-4.4,0.,30.4));
#14220=CARTESIAN_POINT('',(-4.675,-3.36777869765523E-17,30.5));
#14221=CARTESIAN_POINT('Origin',(-4.4,0.,30.5));
#14222=CARTESIAN_POINT('',(-4.675,3.36777869765523E-17,31.5));
#14223=CARTESIAN_POINT('',(-4.675,-3.36777869765523E-17,30.4));
#14224=CARTESIAN_POINT('Origin',(-4.4,0.,31.5));
#14225=CARTESIAN_POINT('Origin',(9.5,10.,30.4));
#14226=CARTESIAN_POINT('',(9.225,10.,30.5));
#14227=CARTESIAN_POINT('Origin',(9.5,10.,30.5));
#14228=CARTESIAN_POINT('',(9.225,10.,31.5));
#14229=CARTESIAN_POINT('',(9.225,10.,30.4));
#14230=CARTESIAN_POINT('Origin',(9.5,10.,31.5));
#14231=CARTESIAN_POINT('Origin',(9.5,11.,30.4));
#14232=CARTESIAN_POINT('',(9.225,11.,30.5));
#14233=CARTESIAN_POINT('Origin',(9.5,11.,30.5));
#14234=CARTESIAN_POINT('',(9.225,11.,31.5));
#14235=CARTESIAN_POINT('',(9.225,11.,30.4));
#14236=CARTESIAN_POINT('Origin',(9.5,11.,31.5));
#14237=CARTESIAN_POINT('Origin',(-9.5,10.,30.4));
#14238=CARTESIAN_POINT('',(-9.775,10.,30.5));
#14239=CARTESIAN_POINT('Origin',(-9.5,10.,30.5));
#14240=CARTESIAN_POINT('',(-9.775,10.,31.5));
#14241=CARTESIAN_POINT('',(-9.775,10.,30.4));
#14242=CARTESIAN_POINT('Origin',(-9.5,10.,31.5));
#14243=CARTESIAN_POINT('Origin',(-9.5,11.,30.4));
#14244=CARTESIAN_POINT('',(-9.775,11.,30.5));
#14245=CARTESIAN_POINT('Origin',(-9.5,11.,30.5));
#14246=CARTESIAN_POINT('',(-9.775,11.,31.5));
#14247=CARTESIAN_POINT('',(-9.775,11.,30.4));
#14248=CARTESIAN_POINT('Origin',(-9.5,11.,31.5));
#14249=CARTESIAN_POINT('Origin',(6.,-4.,30.4));
#14250=CARTESIAN_POINT('',(5.39,-4.,30.5));
#14251=CARTESIAN_POINT('Origin',(6.,-4.,30.5));
#14252=CARTESIAN_POINT('',(5.39,-4.,31.5));
#14253=CARTESIAN_POINT('',(5.39,-4.,30.4));
#14254=CARTESIAN_POINT('Origin',(6.,-4.,31.5));
#14255=CARTESIAN_POINT('Origin',(-6.,4.,30.4));
#14256=CARTESIAN_POINT('',(-6.61,4.,30.5));
#14257=CARTESIAN_POINT('Origin',(-6.,4.,30.5));
#14258=CARTESIAN_POINT('',(-6.61,4.,31.5));
#14259=CARTESIAN_POINT('',(-6.61,4.,30.4));
#14260=CARTESIAN_POINT('Origin',(-6.,4.,31.5));
#14261=CARTESIAN_POINT('Origin',(-6.,-4.,30.4));
#14262=CARTESIAN_POINT('',(-6.61,-4.,30.5));
#14263=CARTESIAN_POINT('Origin',(-6.,-4.,30.5));
#14264=CARTESIAN_POINT('',(-6.61,-4.,31.5));
#14265=CARTESIAN_POINT('',(-6.61,-4.,30.4));
#14266=CARTESIAN_POINT('Origin',(-6.,-4.,31.5));
#14267=CARTESIAN_POINT('Origin',(6.,4.,30.4));
#14268=CARTESIAN_POINT('',(5.39,4.,30.5));
#14269=CARTESIAN_POINT('Origin',(6.,4.,30.5));
#14270=CARTESIAN_POINT('',(5.39,4.,31.5));
#14271=CARTESIAN_POINT('',(5.39,4.,30.4));
#14272=CARTESIAN_POINT('Origin',(6.,4.,31.5));
#14273=CARTESIAN_POINT('Origin',(10.5,11.5,30.5));
#14274=CARTESIAN_POINT('',(10.5,11.5,30.5));
#14275=CARTESIAN_POINT('',(-10.5,11.5,30.5));
#14276=CARTESIAN_POINT('',(10.5,11.5,30.5));
#14277=CARTESIAN_POINT('',(-10.5,11.5,31.5));
#14278=CARTESIAN_POINT('',(-10.5,11.5,30.5));
#14279=CARTESIAN_POINT('',(10.5,11.5,31.5));
#14280=CARTESIAN_POINT('',(10.5,11.5,31.5));
#14281=CARTESIAN_POINT('',(10.5,11.5,30.5));
#14282=CARTESIAN_POINT('Origin',(10.5,-8.,30.5));
#14283=CARTESIAN_POINT('',(10.5,-8.,30.5));
#14284=CARTESIAN_POINT('',(10.5,-8.,30.5));
#14285=CARTESIAN_POINT('',(10.5,-8.,31.5));
#14286=CARTESIAN_POINT('',(10.5,-8.,31.5));
#14287=CARTESIAN_POINT('',(10.5,-8.,30.5));
#14288=CARTESIAN_POINT('Origin',(-10.5,-8.,30.5));
#14289=CARTESIAN_POINT('',(-10.5,-8.,30.5));
#14290=CARTESIAN_POINT('',(-10.5,-8.,30.5));
#14291=CARTESIAN_POINT('',(-10.5,-8.,31.5));
#14292=CARTESIAN_POINT('',(-10.5,-8.,31.5));
#14293=CARTESIAN_POINT('',(-10.5,-8.,30.5));
#14294=CARTESIAN_POINT('Origin',(-10.5,11.5,30.5));
#14295=CARTESIAN_POINT('',(-10.5,11.5,30.5));
#14296=CARTESIAN_POINT('',(-10.5,11.5,31.5));
#14297=CARTESIAN_POINT('Origin',(0.,1.75,31.5));
#14298=CARTESIAN_POINT('Origin',(0.,1.75,30.5));
#14299=CARTESIAN_POINT('',(0.,0.,0.));
#14300=CARTESIAN_POINT('Origin',(-9.5,10.,29.4));
#14301=CARTESIAN_POINT('',(-9.71,10.,29.4));
#14302=CARTESIAN_POINT('Origin',(-9.5,10.,29.4));
#14303=CARTESIAN_POINT('',(-9.71,10.,30.5));
#14304=CARTESIAN_POINT('',(-9.71,10.,29.4));
#14305=CARTESIAN_POINT('Origin',(-9.5,10.,30.5));
#14306=CARTESIAN_POINT('Origin',(-9.5,10.,29.4));
#14307=CARTESIAN_POINT('Origin',(-9.5,11.,29.4));
#14308=CARTESIAN_POINT('',(-9.71,11.,29.4));
#14309=CARTESIAN_POINT('Origin',(-9.5,11.,29.4));
#14310=CARTESIAN_POINT('',(-9.71,11.,30.5));
#14311=CARTESIAN_POINT('',(-9.71,11.,29.4));
#14312=CARTESIAN_POINT('Origin',(-9.5,11.,30.5));
#14313=CARTESIAN_POINT('Origin',(-9.5,11.,29.4));
#14314=CARTESIAN_POINT('Origin',(-9.5,10.,-0.1));
#14315=CARTESIAN_POINT('',(-9.71,10.,0.));
#14316=CARTESIAN_POINT('Origin',(-9.5,10.,0.));
#14317=CARTESIAN_POINT('',(-9.71,10.,1.1));
#14318=CARTESIAN_POINT('',(-9.71,10.,-0.1));
#14319=CARTESIAN_POINT('Origin',(-9.5,10.,1.1));
#14320=CARTESIAN_POINT('Origin',(-9.5,10.,1.1));
#14321=CARTESIAN_POINT('Origin',(-9.5,11.,-0.1));
#14322=CARTESIAN_POINT('',(-9.71,11.,0.));
#14323=CARTESIAN_POINT('Origin',(-9.5,11.,0.));
#14324=CARTESIAN_POINT('',(-9.71,11.,1.1));
#14325=CARTESIAN_POINT('',(-9.71,11.,-0.1));
#14326=CARTESIAN_POINT('Origin',(-9.5,11.,1.1));
#14327=CARTESIAN_POINT('Origin',(-9.5,11.,1.1));
#14328=CARTESIAN_POINT('Origin',(-9.,11.5,0.));
#14329=CARTESIAN_POINT('',(-9.,11.5,0.));
#14330=CARTESIAN_POINT('',(-10.,11.5,0.));
#14331=CARTESIAN_POINT('',(-9.,11.5,0.));
#14332=CARTESIAN_POINT('',(-10.,11.5,30.5));
#14333=CARTESIAN_POINT('',(-10.,11.5,0.));
#14334=CARTESIAN_POINT('',(-9.,11.5,30.5));
#14335=CARTESIAN_POINT('',(-9.,11.5,30.5));
#14336=CARTESIAN_POINT('',(-9.,11.5,0.));
#14337=CARTESIAN_POINT('Origin',(-9.,9.5,0.));
#14338=CARTESIAN_POINT('',(-9.,9.5,0.));
#14339=CARTESIAN_POINT('',(-9.,9.5,0.));
#14340=CARTESIAN_POINT('',(-9.,9.5,30.5));
#14341=CARTESIAN_POINT('',(-9.,9.5,30.5));
#14342=CARTESIAN_POINT('',(-9.,9.5,0.));
#14343=CARTESIAN_POINT('Origin',(-10.,9.5,0.));
#14344=CARTESIAN_POINT('',(-10.,9.5,0.));
#14345=CARTESIAN_POINT('',(-10.,9.5,0.));
#14346=CARTESIAN_POINT('',(-10.,9.5,30.5));
#14347=CARTESIAN_POINT('',(-10.,9.5,30.5));
#14348=CARTESIAN_POINT('',(-10.,9.5,0.));
#14349=CARTESIAN_POINT('Origin',(-10.,11.5,0.));
#14350=CARTESIAN_POINT('',(-10.,11.5,0.));
#14351=CARTESIAN_POINT('',(-10.,11.5,30.5));
#14352=CARTESIAN_POINT('Origin',(-9.5,10.5,30.5));
#14353=CARTESIAN_POINT('Origin',(-9.5,10.5,0.));
#14354=CARTESIAN_POINT('',(0.,0.,0.));
#14355=CARTESIAN_POINT('Origin',(9.5,10.,29.4));
#14356=CARTESIAN_POINT('',(9.29,10.,29.4));
#14357=CARTESIAN_POINT('Origin',(9.5,10.,29.4));
#14358=CARTESIAN_POINT('',(9.29,10.,30.5));
#14359=CARTESIAN_POINT('',(9.29,10.,29.4));
#14360=CARTESIAN_POINT('Origin',(9.5,10.,30.5));
#14361=CARTESIAN_POINT('Origin',(9.5,10.,29.4));
#14362=CARTESIAN_POINT('Origin',(9.5,11.,29.4));
#14363=CARTESIAN_POINT('',(9.29,11.,29.4));
#14364=CARTESIAN_POINT('Origin',(9.5,11.,29.4));
#14365=CARTESIAN_POINT('',(9.29,11.,30.5));
#14366=CARTESIAN_POINT('',(9.29,11.,29.4));
#14367=CARTESIAN_POINT('Origin',(9.5,11.,30.5));
#14368=CARTESIAN_POINT('Origin',(9.5,11.,29.4));
#14369=CARTESIAN_POINT('Origin',(9.5,10.,-0.1));
#14370=CARTESIAN_POINT('',(9.29,10.,0.));
#14371=CARTESIAN_POINT('Origin',(9.5,10.,0.));
#14372=CARTESIAN_POINT('',(9.29,10.,1.1));
#14373=CARTESIAN_POINT('',(9.29,10.,-0.1));
#14374=CARTESIAN_POINT('Origin',(9.5,10.,1.1));
#14375=CARTESIAN_POINT('Origin',(9.5,10.,1.1));
#14376=CARTESIAN_POINT('Origin',(9.5,11.,-0.1));
#14377=CARTESIAN_POINT('',(9.29,11.,0.));
#14378=CARTESIAN_POINT('Origin',(9.5,11.,0.));
#14379=CARTESIAN_POINT('',(9.29,11.,1.1));
#14380=CARTESIAN_POINT('',(9.29,11.,-0.1));
#14381=CARTESIAN_POINT('Origin',(9.5,11.,1.1));
#14382=CARTESIAN_POINT('Origin',(9.5,11.,1.1));
#14383=CARTESIAN_POINT('Origin',(10.,11.5,0.));
#14384=CARTESIAN_POINT('',(10.,11.5,0.));
#14385=CARTESIAN_POINT('',(9.,11.5,0.));
#14386=CARTESIAN_POINT('',(10.,11.5,0.));
#14387=CARTESIAN_POINT('',(9.,11.5,30.5));
#14388=CARTESIAN_POINT('',(9.,11.5,0.));
#14389=CARTESIAN_POINT('',(10.,11.5,30.5));
#14390=CARTESIAN_POINT('',(10.,11.5,30.5));
#14391=CARTESIAN_POINT('',(10.,11.5,0.));
#14392=CARTESIAN_POINT('Origin',(10.,9.5,0.));
#14393=CARTESIAN_POINT('',(10.,9.5,0.));
#14394=CARTESIAN_POINT('',(10.,9.5,0.));
#14395=CARTESIAN_POINT('',(10.,9.5,30.5));
#14396=CARTESIAN_POINT('',(10.,9.5,30.5));
#14397=CARTESIAN_POINT('',(10.,9.5,0.));
#14398=CARTESIAN_POINT('Origin',(9.,9.5,0.));
#14399=CARTESIAN_POINT('',(9.,9.5,0.));
#14400=CARTESIAN_POINT('',(9.,9.5,0.));
#14401=CARTESIAN_POINT('',(9.,9.5,30.5));
#14402=CARTESIAN_POINT('',(9.,9.5,30.5));
#14403=CARTESIAN_POINT('',(9.,9.5,0.));
#14404=CARTESIAN_POINT('Origin',(9.,11.5,0.));
#14405=CARTESIAN_POINT('',(9.,11.5,0.));
#14406=CARTESIAN_POINT('',(9.,11.5,30.5));
#14407=CARTESIAN_POINT('Origin',(9.5,10.5,30.5));
#14408=CARTESIAN_POINT('Origin',(9.5,10.5,0.));
#14409=CARTESIAN_POINT('',(0.,0.,0.));
#14410=CARTESIAN_POINT('Origin',(-7.6,-1.3,-0.1));
#14411=CARTESIAN_POINT('',(-7.81,-1.3,0.));
#14412=CARTESIAN_POINT('Origin',(-7.6,-1.3,0.));
#14413=CARTESIAN_POINT('',(-7.81,-1.3,0.9));
#14414=CARTESIAN_POINT('',(-7.81,-1.3,-0.1));
#14415=CARTESIAN_POINT('Origin',(-7.6,-1.3,0.9));
#14416=CARTESIAN_POINT('Origin',(-7.6,-1.3,0.9));
#14417=CARTESIAN_POINT('Origin',(-4.4,-1.3,-0.1));
#14418=CARTESIAN_POINT('',(-4.61,-1.3,0.));
#14419=CARTESIAN_POINT('Origin',(-4.4,-1.3,0.));
#14420=CARTESIAN_POINT('',(-4.61,-1.3,0.9));
#14421=CARTESIAN_POINT('',(-4.61,-1.3,-0.1));
#14422=CARTESIAN_POINT('Origin',(-4.4,-1.3,0.9));
#14423=CARTESIAN_POINT('Origin',(-4.4,-1.3,0.9));
#14424=CARTESIAN_POINT('Origin',(-7.6,-1.8,1.2));
#14425=CARTESIAN_POINT('',(-7.81,-1.7,1.2));
#14426=CARTESIAN_POINT('Origin',(-7.6,-1.7,1.2));
#14427=CARTESIAN_POINT('',(-7.81,-0.9,1.2));
#14428=CARTESIAN_POINT('',(-7.81,-1.8,1.2));
#14429=CARTESIAN_POINT('Origin',(-7.6,-0.9,1.2));
#14430=CARTESIAN_POINT('Origin',(-4.4,-1.8,1.2));
#14431=CARTESIAN_POINT('',(-4.61,-1.7,1.2));
#14432=CARTESIAN_POINT('Origin',(-4.4,-1.7,1.2));
#14433=CARTESIAN_POINT('',(-4.61,-0.9,1.2));
#14434=CARTESIAN_POINT('',(-4.61,-1.8,1.2));
#14435=CARTESIAN_POINT('Origin',(-4.4,-0.9,1.2));
#14436=CARTESIAN_POINT('Origin',(-3.6,-0.9,0.));
#14437=CARTESIAN_POINT('',(-3.6,-0.9,0.));
#14438=CARTESIAN_POINT('',(-8.4,-0.9,0.));
#14439=CARTESIAN_POINT('',(-3.6,-0.9,0.));
#14440=CARTESIAN_POINT('',(-8.4,-0.9,3.));
#14441=CARTESIAN_POINT('',(-8.4,-0.9,0.));
#14442=CARTESIAN_POINT('',(-3.6,-0.9,3.));
#14443=CARTESIAN_POINT('',(-3.6,-0.9,3.));
#14444=CARTESIAN_POINT('',(-3.6,-0.9,0.));
#14445=CARTESIAN_POINT('Origin',(-3.6,-1.7,0.));
#14446=CARTESIAN_POINT('',(-3.6,-1.7,0.));
#14447=CARTESIAN_POINT('',(-3.6,-1.7,0.));
#14448=CARTESIAN_POINT('',(-3.6,-1.7,3.));
#14449=CARTESIAN_POINT('',(-3.6,-1.7,3.));
#14450=CARTESIAN_POINT('',(-3.6,-1.7,0.));
#14451=CARTESIAN_POINT('Origin',(-8.4,-1.7,0.));
#14452=CARTESIAN_POINT('',(-8.4,-1.7,0.));
#14453=CARTESIAN_POINT('',(-8.4,-1.7,0.));
#14454=CARTESIAN_POINT('',(-8.4,-1.7,3.));
#14455=CARTESIAN_POINT('',(-8.4,-1.7,3.));
#14456=CARTESIAN_POINT('',(-8.4,-1.7,0.));
#14457=CARTESIAN_POINT('Origin',(-8.4,-0.9,0.));
#14458=CARTESIAN_POINT('',(-8.4,-0.9,0.));
#14459=CARTESIAN_POINT('',(-8.4,-0.9,3.));
#14460=CARTESIAN_POINT('Origin',(-6.,-1.3,3.));
#14461=CARTESIAN_POINT('Origin',(-6.,-1.3,0.));
#14462=CARTESIAN_POINT('',(0.,0.,0.));
#14463=CARTESIAN_POINT('Origin',(-7.6,0.,29.6));
#14464=CARTESIAN_POINT('',(-7.81,-2.57175827820944E-17,29.7));
#14465=CARTESIAN_POINT('Origin',(-7.6,0.,29.7));
#14466=CARTESIAN_POINT('',(-7.81,2.57175827820944E-17,30.5));
#14467=CARTESIAN_POINT('',(-7.81,-2.57175827820944E-17,29.6));
#14468=CARTESIAN_POINT('Origin',(-7.6,0.,30.5));
#14469=CARTESIAN_POINT('Origin',(-4.4,0.,29.6));
#14470=CARTESIAN_POINT('',(-4.61,-2.57175827820944E-17,29.7));
#14471=CARTESIAN_POINT('Origin',(-4.4,0.,29.7));
#14472=CARTESIAN_POINT('',(-4.61,2.57175827820944E-17,30.5));
#14473=CARTESIAN_POINT('',(-4.61,-2.57175827820944E-17,29.6));
#14474=CARTESIAN_POINT('Origin',(-4.4,0.,30.5));
#14475=CARTESIAN_POINT('Origin',(-7.6,-1.8,29.8));
#14476=CARTESIAN_POINT('',(-7.81,-1.7,29.8));
#14477=CARTESIAN_POINT('Origin',(-7.6,-1.7,29.8));
#14478=CARTESIAN_POINT('',(-7.81,-0.8,29.8));
#14479=CARTESIAN_POINT('',(-7.81,-1.8,29.8));
#14480=CARTESIAN_POINT('',(-7.41533814687381,-0.8,29.7));
#14481=CARTESIAN_POINT('Origin',(-7.6,-0.8,29.8));
#14482=CARTESIAN_POINT('',(-7.4153381468738,-0.9,29.7));
#14483=CARTESIAN_POINT('',(-7.41533814687381,-1.8,29.7));
#14484=CARTESIAN_POINT('',(-7.78466185312619,-0.9,29.7));
#14485=CARTESIAN_POINT('Origin',(-7.6,-0.9,29.8));
#14486=CARTESIAN_POINT('',(-7.78466185312619,-0.8,29.7));
#14487=CARTESIAN_POINT('',(-7.78466185312619,-1.8,29.7));
#14488=CARTESIAN_POINT('Origin',(-7.6,-0.8,29.8));
#14489=CARTESIAN_POINT('Origin',(-7.6,-0.8,29.8));
#14490=CARTESIAN_POINT('',(-5.6,-0.8,29.7));
#14491=CARTESIAN_POINT('Origin',(-4.4,-1.8,29.8));
#14492=CARTESIAN_POINT('',(-4.61,-1.7,29.8));
#14493=CARTESIAN_POINT('Origin',(-4.4,-1.7,29.8));
#14494=CARTESIAN_POINT('',(-4.61,-0.8,29.8));
#14495=CARTESIAN_POINT('',(-4.61,-1.8,29.8));
#14496=CARTESIAN_POINT('',(-4.21533814687381,-0.8,29.7));
#14497=CARTESIAN_POINT('Origin',(-4.4,-0.8,29.8));
#14498=CARTESIAN_POINT('',(-4.21533814687381,-0.9,29.7));
#14499=CARTESIAN_POINT('',(-4.21533814687381,-1.8,29.7));
#14500=CARTESIAN_POINT('',(-4.5846618531262,-0.9,29.7));
#14501=CARTESIAN_POINT('Origin',(-4.4,-0.9,29.8));
#14502=CARTESIAN_POINT('',(-4.58466185312619,-0.8,29.7));
#14503=CARTESIAN_POINT('',(-4.58466185312619,-1.8,29.7));
#14504=CARTESIAN_POINT('Origin',(-4.4,-0.8,29.8));
#14505=CARTESIAN_POINT('Origin',(-4.4,-0.8,29.8));
#14506=CARTESIAN_POINT('',(-4.,-0.8,29.7));
#14507=CARTESIAN_POINT('Origin',(-3.6,-0.9,28.));
#14508=CARTESIAN_POINT('',(-3.6,-0.9,29.7));
#14509=CARTESIAN_POINT('',(-3.6,-0.9,29.7));
#14510=CARTESIAN_POINT('',(-3.6,-0.9,29.7));
#14511=CARTESIAN_POINT('',(-3.6,-0.9,28.));
#14512=CARTESIAN_POINT('',(-3.6,-0.9,28.));
#14513=CARTESIAN_POINT('',(-8.4,-0.9,28.));
#14514=CARTESIAN_POINT('',(-3.6,-0.9,28.));
#14515=CARTESIAN_POINT('',(-8.4,-0.9,29.7));
#14516=CARTESIAN_POINT('',(-8.4,-0.9,28.));
#14517=CARTESIAN_POINT('',(-3.6,-0.9,29.7));
#14518=CARTESIAN_POINT('Origin',(-3.6,-1.7,29.7));
#14519=CARTESIAN_POINT('',(-8.4,1.,29.7));
#14520=CARTESIAN_POINT('',(-8.4,-1.7,29.7));
#14521=CARTESIAN_POINT('',(-3.6,1.,29.7));
#14522=CARTESIAN_POINT('',(-8.4,1.,29.7));
#14523=CARTESIAN_POINT('',(-3.6,-1.7,29.7));
#14524=CARTESIAN_POINT('Origin',(-6.,1.,30.1));
#14525=CARTESIAN_POINT('',(-8.4,1.,30.5));
#14526=CARTESIAN_POINT('',(-3.6,1.,30.5));
#14527=CARTESIAN_POINT('',(-3.6,1.,30.5));
#14528=CARTESIAN_POINT('',(-3.6,1.,29.7));
#14529=CARTESIAN_POINT('',(-8.4,1.,30.5));
#14530=CARTESIAN_POINT('Origin',(-3.6,-1.7,28.));
#14531=CARTESIAN_POINT('',(-3.6,-1.7,28.));
#14532=CARTESIAN_POINT('',(-3.6,-1.7,30.5));
#14533=CARTESIAN_POINT('',(-3.6,-1.7,28.));
#14534=CARTESIAN_POINT('',(-3.6,-1.7,28.));
#14535=CARTESIAN_POINT('',(-3.6,-1.7,30.5));
#14536=CARTESIAN_POINT('Origin',(-8.4,-1.7,28.));
#14537=CARTESIAN_POINT('',(-8.4,-1.7,28.));
#14538=CARTESIAN_POINT('',(-8.4,-1.7,30.5));
#14539=CARTESIAN_POINT('',(-8.4,-1.7,28.));
#14540=CARTESIAN_POINT('',(-8.4,-1.7,28.));
#14541=CARTESIAN_POINT('',(-8.4,-1.7,30.5));
#14542=CARTESIAN_POINT('Origin',(-8.4,-0.9,28.));
#14543=CARTESIAN_POINT('',(-8.4,-0.9,28.));
#14544=CARTESIAN_POINT('',(-8.4,-1.7,30.5));
#14545=CARTESIAN_POINT('Origin',(-6.,-1.3,30.5));
#14546=CARTESIAN_POINT('Origin',(-6.,-1.3,28.));
#14547=CARTESIAN_POINT('',(0.,0.,0.));
#14548=CARTESIAN_POINT('Origin',(-6.,-4.,1.9));
#14549=CARTESIAN_POINT('',(-6.625,-4.,2.6));
#14550=CARTESIAN_POINT('Origin',(-6.,-4.,2.6));
#14551=CARTESIAN_POINT('',(-6.625,-4.,1.9));
#14552=CARTESIAN_POINT('',(-6.625,-4.,1.9));
#14553=CARTESIAN_POINT('Origin',(-6.,-4.,1.9));
#14554=CARTESIAN_POINT('Origin',(-6.,-4.,1.9));
#14555=CARTESIAN_POINT('',(-7.5,-4.,2.6));
#14556=CARTESIAN_POINT('Origin',(-6.,-4.,2.6));
#14557=CARTESIAN_POINT('',(-7.5,-4.,1.9));
#14558=CARTESIAN_POINT('',(-7.5,-4.,1.9));
#14559=CARTESIAN_POINT('Origin',(-6.,-4.,1.9));
#14560=CARTESIAN_POINT('Origin',(-6.,-4.,2.6));
#14561=CARTESIAN_POINT('Origin',(-6.,-4.,1.9));
#14562=CARTESIAN_POINT('',(0.,0.,0.));
#14563=CARTESIAN_POINT('Ctrl Pts',(-5.0000018410068,-3.98632452652701,2.60093950625047));
#14564=CARTESIAN_POINT('Ctrl Pts',(-5.00002711936198,-3.79855038268961,
2.62686205390092));
#14565=CARTESIAN_POINT('Ctrl Pts',(-5.10766548646186,-3.42414266353048,
2.67881373981085));
#14566=CARTESIAN_POINT('Ctrl Pts',(-5.54728618664091,-3.02997941177219,
2.75738438838345));
#14567=CARTESIAN_POINT('Ctrl Pts',(-6.13328094577175,-2.93005881251319,
2.83651316903494));
#14568=CARTESIAN_POINT('Ctrl Pts',(-6.68670283260197,-3.15858336118752,
2.91622304878198));
#14569=CARTESIAN_POINT('Ctrl Pts',(-7.03616187921695,-3.65012597802659,
2.99648821676135));
#14570=CARTESIAN_POINT('Ctrl Pts',(-7.07062949516082,-4.25616589762635,
3.07729930317819));
#14571=CARTESIAN_POINT('Ctrl Pts',(-6.77580863517498,-4.79139923899731,
3.15863489698049));
#14572=CARTESIAN_POINT('Ctrl Pts',(-6.23777999713871,-5.08919902934938,
3.24047455745509));
#14573=CARTESIAN_POINT('Ctrl Pts',(-5.62032344264714,-5.05504677509261,
3.32279321070673));
#14574=CARTESIAN_POINT('Ctrl Pts',(-5.11287137916696,-4.69557478020053,
3.40556356877954));
#14575=CARTESIAN_POINT('Ctrl Pts',(-4.87329914702911,-4.11831903637453,
3.48875540125931));
#14576=CARTESIAN_POINT('Ctrl Pts',(-4.97807346419814,-3.49920456570944,
3.57233609900605));
#14577=CARTESIAN_POINT('Ctrl Pts',(-5.39799493781825,-3.02877333945258,
3.65627071903615));
#14578=CARTESIAN_POINT('Ctrl Pts',(-6.00610273172108,-2.85326324045065,
3.74052224127624));
#14579=CARTESIAN_POINT('Ctrl Pts',(-6.61643757836359,-3.02876545098225,
3.82505176791358));
#14580=CARTESIAN_POINT('Ctrl Pts',(-7.02513160270699,-3.48597574268572,
3.90667922493066));
#14581=CARTESIAN_POINT('Ctrl Pts',(-7.12235641775929,-3.9685483460108,3.97275270898905));
#14582=CARTESIAN_POINT('Ctrl Pts',(-7.06636481269846,-4.28466100128236,
4.01685604551847));
#14583=CARTESIAN_POINT('Ctrl Pts',(-7.00182040328561,-4.45530975229043,
4.04207155819959));
#14584=CARTESIAN_POINT('Ctrl Pts',(-6.87402691871924,-4.69744869614318,
4.07990746733096));
#14585=CARTESIAN_POINT('Ctrl Pts',(-6.57124878899927,-4.99309357202046,
4.1367051149187));
#14586=CARTESIAN_POINT('Ctrl Pts',(-6.02768033690931,-5.14605913758532,
4.2124974864954));
#14587=CARTESIAN_POINT('Ctrl Pts',(-5.47679456345111,-5.0204436702095,4.28832048286543));
#14588=CARTESIAN_POINT('Ctrl Pts',(-5.08889541312948,-4.67743201497751,
4.35782392862843));
#14589=CARTESIAN_POINT('Ctrl Pts',(-4.90355272665998,-4.25185719379132,
4.42098501738742));
#14590=CARTESIAN_POINT('Ctrl Pts',(-4.88772422317122,-3.83457870292561,
4.47779828347438));
#14591=CARTESIAN_POINT('Ctrl Pts',(-5.02577825319216,-3.44096047951616,
4.5345666000236));
#14592=CARTESIAN_POINT('Ctrl Pts',(-5.32758243531257,-3.08955719770179,
4.59757801626674));
#14593=CARTESIAN_POINT('Ctrl Pts',(-5.79757132369034,-2.87764760865861,
4.66678930745632));
#14594=CARTESIAN_POINT('Ctrl Pts',(-6.35748141231083,-2.91980778121556,
4.74213608943437));
#14595=CARTESIAN_POINT('Ctrl Pts',(-6.72958410590507,-3.16055362161142,
4.80163845366161));
#14596=CARTESIAN_POINT('Ctrl Pts',(-6.922583408066,-3.41255717151317,4.8453962925926));
#14597=CARTESIAN_POINT('Ctrl Pts',(-7.04520229026909,-3.65506744231538,
4.88286085267916));
#14598=CARTESIAN_POINT('Ctrl Pts',(-7.10903827020174,-3.9926759490213,4.92960885619655));
#14599=CARTESIAN_POINT('Ctrl Pts',(-7.032354492376,-4.39667067923105,4.98556279568034));
#14600=CARTESIAN_POINT('Ctrl Pts',(-6.81415974257675,-4.74396102273289,
5.04136211338037));
#14601=CARTESIAN_POINT('Ctrl Pts',(-6.48510242262688,-4.98648342248571,
5.09699623581333));
#14602=CARTESIAN_POINT('Ctrl Pts',(-6.09122164110091,-5.09213718968761,
5.15245506498449));
#14603=CARTESIAN_POINT('Ctrl Pts',(-5.6879156360413,-5.04618557814476,5.20772889788153));
#14604=CARTESIAN_POINT('Ctrl Pts',(-5.20960410281967,-4.79482820495352,
5.28116853491036));
#14605=CARTESIAN_POINT('Ctrl Pts',(-4.85635661256684,-4.18339627204868,
5.37246079310469));
#14606=CARTESIAN_POINT('Ctrl Pts',(-5.04534497366866,-3.36152922837358,
5.4811368047244));
#14607=CARTESIAN_POINT('Ctrl Pts',(-5.62045222073828,-2.97210695679973,
5.57092649482181));
#14608=CARTESIAN_POINT('Ctrl Pts',(-6.14491401311764,-2.95446524901901,
5.64227218329944));
#14609=CARTESIAN_POINT('Ctrl Pts',(-6.55538629310792,-3.09741218079302,
5.70145206897501));
#14610=CARTESIAN_POINT('Ctrl Pts',(-6.90061904209687,-3.43455608810828,
5.76619150175189));
#14611=CARTESIAN_POINT('Ctrl Pts',(-7.05403180026006,-3.93434682913999,
5.83636208061574));
#14612=CARTESIAN_POINT('Ctrl Pts',(-6.95084370870626,-4.44331194962687,
5.90607316768221));
#14613=CARTESIAN_POINT('Ctrl Pts',(-6.61884201115902,-4.83828819326241,
5.97532164622816));
#14614=CARTESIAN_POINT('Ctrl Pts',(-6.14163977231472,-5.02507153362565,
6.04410658214742));
#14615=CARTESIAN_POINT('Ctrl Pts',(-5.67874308979945,-4.96670943531882,
6.10673565115305));
#14616=CARTESIAN_POINT('Ctrl Pts',(-5.32673727495899,-4.74487796933182,
6.16333654805419));
#14617=CARTESIAN_POINT('Ctrl Pts',(-5.10557737295403,-4.44521639081723,
6.21402149420468));
#14618=CARTESIAN_POINT('Ctrl Pts',(-5.00986236436416,-4.08706033297606,
6.26445344628883));
#14619=CARTESIAN_POINT('Ctrl Pts',(-5.05132140869747,-3.72058500062059,
6.31463598386295));
#14620=CARTESIAN_POINT('Ctrl Pts',(-5.22295427342147,-3.39619318419661,
6.36457331207659));
#14621=CARTESIAN_POINT('Ctrl Pts',(-5.49996349858563,-3.15797332202467,
6.41427030413784));
#14622=CARTESIAN_POINT('Ctrl Pts',(-5.843023257891,-3.03825996963253,6.46373244033231));
#14623=CARTESIAN_POINT('Ctrl Pts',(-6.2651798733637,-3.05368284090179,6.52117143934356));
#14624=CARTESIAN_POINT('Ctrl Pts',(-6.69395218073661,-3.29085487418832,
6.58644589644131));
#14625=CARTESIAN_POINT('Ctrl Pts',(-6.9588514090406,-3.77142724594311,6.65940509135759));
#14626=CARTESIAN_POINT('Ctrl Pts',(-6.93289301903251,-4.22410112506723,
6.71983222544231));
#14627=CARTESIAN_POINT('Ctrl Pts',(-6.77106481048377,-4.53615877260298,
6.76796591761938));
#14628=CARTESIAN_POINT('Ctrl Pts',(-6.57088599598262,-4.74749645053629,
6.8079662999785));
#14629=CARTESIAN_POINT('Ctrl Pts',(-6.18196007039062,-4.95496402481898,
6.86778079666891));
#14630=CARTESIAN_POINT('Ctrl Pts',(-5.63200940413013,-4.91297894303413,
6.93919834468442));
#14631=CARTESIAN_POINT('Ctrl Pts',(-5.18963313111942,-4.51545599119052,
7.01814869825501));
#14632=CARTESIAN_POINT('Ctrl Pts',(-5.04266994609727,-4.00519996765647,
7.08893288548598));
#14633=CARTESIAN_POINT('Ctrl Pts',(-5.18994160065279,-3.49569082009585,
7.15948665627275));
#14634=CARTESIAN_POINT('Ctrl Pts',(-5.58406477811046,-3.14370617953113,
7.22985222522876));
#14635=CARTESIAN_POINT('Ctrl Pts',(-6.10419876841606,-3.05543002721108,
7.30007283323036));
#14636=CARTESIAN_POINT('Ctrl Pts',(-6.59085610258569,-3.25712241290123,
7.37019262147636));
#14637=CARTESIAN_POINT('Ctrl Pts',(-6.8952969281062,-3.68642062054244,7.44025632508636));
#14638=CARTESIAN_POINT('Ctrl Pts',(-6.92507910037993,-4.2118623997588,7.51030900497373));
#14639=CARTESIAN_POINT('Ctrl Pts',(-6.67029196164112,-4.6727438878236,7.58039577683535));
#14640=CARTESIAN_POINT('Ctrl Pts',(-6.20902606294958,-4.92782413963266,
7.65056157433059));
#14641=CARTESIAN_POINT('Ctrl Pts',(-5.68175068955988,-4.89838259463549,
7.72085085746158));
#14642=CARTESIAN_POINT('Ctrl Pts',(-5.24995696526907,-4.59224234497362,
7.79130734612191));
#14643=CARTESIAN_POINT('Ctrl Pts',(-5.04653976812282,-4.10189023096155,
7.86197377554524));
#14644=CARTESIAN_POINT('Ctrl Pts',(-5.13553771446182,-3.57654536818086,
7.93289164421975));
#14645=CARTESIAN_POINT('Ctrl Pts',(-5.49167958880606,-3.17757206270347,
8.00410097016463));
#14646=CARTESIAN_POINT('Ctrl Pts',(-6.00820878856796,-3.02820291673281,
8.07564000225066));
#14647=CARTESIAN_POINT('Ctrl Pts',(-6.44062187419601,-3.15261370888403,
8.13556092469148));
#14648=CARTESIAN_POINT('Ctrl Pts',(-6.70861130655355,-3.37965195671477,
8.18369776363854));
#14649=CARTESIAN_POINT('Ctrl Pts',(-6.8937105085998,-3.65581236490976,8.22929135600403));
#14650=CARTESIAN_POINT('Ctrl Pts',(-6.97571459288556,-4.05892831151958,
8.28449961702882));
#14651=CARTESIAN_POINT('Ctrl Pts',(-6.83301647708075,-4.52172879570838,
8.34949564023339));
#14652=CARTESIAN_POINT('Ctrl Pts',(-6.51381452164907,-4.83374162454526,
8.40942447333573));
#14653=CARTESIAN_POINT('Ctrl Pts',(-6.13367096105595,-4.96658596055631,
8.46419547642941));
#14654=CARTESIAN_POINT('Ctrl Pts',(-5.77000769054747,-4.95325944490059,
8.51371979160536));
#14655=CARTESIAN_POINT('Ctrl Pts',(-5.43473421944715,-4.80705755452014,
8.56348049202891));
#14656=CARTESIAN_POINT('Ctrl Pts',(-5.17476962038704,-4.5473411130966,8.6134828902317));
#14657=CARTESIAN_POINT('Ctrl Pts',(-5.02691233865341,-4.20890181210803,
8.66373168353468));
#14658=CARTESIAN_POINT('Ctrl Pts',(-5.01287597198371,-3.83802632501149,
8.71423091550292));
#14659=CARTESIAN_POINT('Ctrl Pts',(-5.13588065841094,-3.48587318149708,
8.76498396862734));
#14660=CARTESIAN_POINT('Ctrl Pts',(-5.38027484984219,-3.20156985271231,
8.81599355960519));
#14661=CARTESIAN_POINT('Ctrl Pts',(-5.71337748308179,-3.0254571982762,8.86726173709343));
#14662=CARTESIAN_POINT('Ctrl Pts',(-6.08966550245643,-2.98274869856715,
8.91878984711541));
#14663=CARTESIAN_POINT('Ctrl Pts',(-6.45733798876018,-3.0812109148485,8.97057858675351));
#14664=CARTESIAN_POINT('Ctrl Pts',(-6.76529910592523,-3.30812336168265,
9.02262792849601));
#14665=CARTESIAN_POINT('Ctrl Pts',(-6.96998046112789,-3.63355675694242,
9.07493719450744));
#14666=CARTESIAN_POINT('Ctrl Pts',(-7.04194989283072,-4.01319995364602,
9.12750500078302));
#14667=CARTESIAN_POINT('Ctrl Pts',(-6.96991048459342,-4.39460760383808,
9.18032929219698));
#14668=CARTESIAN_POINT('Ctrl Pts',(-6.73960211403654,-4.76194359718324,
9.23930488555841));
#14669=CARTESIAN_POINT('Ctrl Pts',(-6.33176853957225,-5.02597941464994,
9.30453505646424));
#14670=CARTESIAN_POINT('Ctrl Pts',(-5.79980377218573,-5.06633098935627,
9.37613051632468));
#14671=CARTESIAN_POINT('Ctrl Pts',(-5.29005475531646,-4.836901018808,9.45115010972279));
#14672=CARTESIAN_POINT('Ctrl Pts',(-4.94827191401131,-4.35650564743655,
9.52964181326016));
#14673=CARTESIAN_POINT('Ctrl Pts',(-4.91327405487842,-3.74129847888372,
9.61164803952703));
#14674=CARTESIAN_POINT('Ctrl Pts',(-5.21254904956895,-3.19880095424663,
9.69412425066449));
#14675=CARTESIAN_POINT('Ctrl Pts',(-5.75755518053287,-2.89705290752891,
9.77704206923956));
#14676=CARTESIAN_POINT('Ctrl Pts',(-6.38261532053777,-2.93174547355756,
9.86037047436186));
#14677=CARTESIAN_POINT('Ctrl Pts',(-6.89571246871018,-3.29533246954376,
9.9440760489684));
#14678=CARTESIAN_POINT('Ctrl Pts',(-7.13766462222267,-3.87856431327716,
10.0281231253342));
#14679=CARTESIAN_POINT('Ctrl Pts',(-7.03181307520858,-4.50336859593469,
10.112474009291));
#14680=CARTESIAN_POINT('Ctrl Pts',(-6.60841405754483,-4.9775421382096,10.1970892234063));
#14681=CARTESIAN_POINT('Ctrl Pts',(-5.99601356400164,-5.15419586953956,
10.2819277209876));
#14682=CARTESIAN_POINT('Ctrl Pts',(-5.38220054085499,-4.97753568370925,
10.3669471364924));
#14683=CARTESIAN_POINT('Ctrl Pts',(-4.95580917322647,-4.50058383383181,
10.4521040148979));
#14684=CARTESIAN_POINT('Ctrl Pts',(-4.84845524689304,-3.86918295104257,
10.5373541217208));
#14685=CARTESIAN_POINT('Ctrl Pts',(-5.09367725879538,-3.27712852401529,
10.6226526455382));
#14686=CARTESIAN_POINT('Ctrl Pts',(-5.6163401918585,-2.90630478068196,10.7079544990261));
#14687=CARTESIAN_POINT('Ctrl Pts',(-6.25592072702474,-2.87046899980689,
10.7932145516894));
#14688=CARTESIAN_POINT('Ctrl Pts',(-6.81586294759382,-3.18009679237689,
10.8783879977619));
#14689=CARTESIAN_POINT('Ctrl Pts',(-7.124955642463,-3.73939634942269,10.963430385322));
#14690=CARTESIAN_POINT('Ctrl Pts',(-7.08867264951758,-4.37593520057008,
11.0482983435205));
#14691=CARTESIAN_POINT('Ctrl Pts',(-6.72062823969146,-4.89450906450982,
11.1329488746335));
#14692=CARTESIAN_POINT('Ctrl Pts',(-6.13472454520284,-5.136799701332,11.217341733611));
#14693=CARTESIAN_POINT('Ctrl Pts',(-5.51200536776972,-5.03087324497862,
11.3014349939178));
#14694=CARTESIAN_POINT('Ctrl Pts',(-5.04306930328679,-4.6109089567958,11.3851957518917));
#14695=CARTESIAN_POINT('Ctrl Pts',(-4.92780437314592,-4.2103503377694,11.4407823887583));
#14696=CARTESIAN_POINT('Ctrl Pts',(-4.92777733020741,-4.00946826990451,
11.4685145081939));
#14697=CARTESIAN_POINT('Ctrl Pts',(-5.02992177076987,-3.98632855437981,
2.60093950625047));
#14698=CARTESIAN_POINT('Ctrl Pts',(-5.02994631566211,-3.80400276249367,
2.62610989942328));
#14699=CARTESIAN_POINT('Ctrl Pts',(-5.13440258778751,-3.44058117095201,
2.67653041943034));
#14700=CARTESIAN_POINT('Ctrl Pts',(-5.56132162600835,-3.05771102958624,
2.75283690301094));
#14701=CARTESIAN_POINT('Ctrl Pts',(-6.13074764302092,-2.96056640229043,
2.82972278836909));
#14702=CARTESIAN_POINT('Ctrl Pts',(-6.66896086911222,-3.1827303900304,2.90723424531236));
#14703=CARTESIAN_POINT('Ctrl Pts',(-7.0091712958513,-3.66112442258111,2.98535323605726));
#14704=CARTESIAN_POINT('Ctrl Pts',(-7.04284600518481,-4.25162088811131,
3.06408757941918));
#14705=CARTESIAN_POINT('Ctrl Pts',(-6.75534616813047,-4.77378941641128,
3.14342203482332));
#14706=CARTESIAN_POINT('Ctrl Pts',(-6.22989350052469,-5.06476181444098,
3.22334341795718));
#14707=CARTESIAN_POINT('Ctrl Pts',(-5.62593684855353,-5.03148535851095,
3.3038501203708));
#14708=CARTESIAN_POINT('Ctrl Pts',(-5.1287541466607,-4.67945429549254,3.38491948457682));
#14709=CARTESIAN_POINT('Ctrl Pts',(-4.89355205236567,-4.11311271692517,
3.46653357829839));
#14710=CARTESIAN_POINT('Ctrl Pts',(-4.99637627302549,-3.50458413255717,
3.54866779717306));
#14711=CARTESIAN_POINT('Ctrl Pts',(-5.40970923759118,-3.04128461772533,
3.63129587938778));
#14712=CARTESIAN_POINT('Ctrl Pts',(-6.00950948085903,-2.867992196767,3.71438836781264));
#14713=CARTESIAN_POINT('Ctrl Pts',(-6.61274600784354,-3.04126505973915,
3.79791226147148));
#14714=CARTESIAN_POINT('Ctrl Pts',(-7.01756958403438,-3.49388616164201,
3.87872583853233));
#14715=CARTESIAN_POINT('Ctrl Pts',(-7.1141315386001,-3.97261134085471,3.9442614338042));
#14716=CARTESIAN_POINT('Ctrl Pts',(-7.05852445971495,-4.28666070323465,
3.98807156329228));
#14717=CARTESIAN_POINT('Ctrl Pts',(-6.99436014221873,-4.45631244072124,
4.01313835147944));
#14718=CARTESIAN_POINT('Ctrl Pts',(-6.86726327177174,-4.69714488722618,
4.05076789045709));
#14719=CARTESIAN_POINT('Ctrl Pts',(-6.56590374625076,-4.99156063284653,
4.10729650412945));
#14720=CARTESIAN_POINT('Ctrl Pts',(-6.02371646768625,-5.14428159346822,
4.18289678502633));
#14721=CARTESIAN_POINT('Ctrl Pts',(-5.47318100169159,-5.01887821754281,
4.25865808314083));
#14722=CARTESIAN_POINT('Ctrl Pts',(-5.08477033821112,-4.67558092229865,
4.32822376669194));
#14723=CARTESIAN_POINT('Ctrl Pts',(-4.89886657854121,-4.24885080118007,
4.39155414030818));
#14724=CARTESIAN_POINT('Ctrl Pts',(-4.88291604792826,-3.82987351104406,
4.44859069874469));
#14725=CARTESIAN_POINT('Ctrl Pts',(-5.02168464637103,-3.43409260120211,
4.50566175306661));
#14726=CARTESIAN_POINT('Ctrl Pts',(-5.32548609673626,-3.08026957325351,
4.56909245555632));
#14727=CARTESIAN_POINT('Ctrl Pts',(-5.79936418578429,-2.86648825136964,
4.63887581219755));
#14728=CARTESIAN_POINT('Ctrl Pts',(-6.36494798765252,-2.90895436286898,
4.71498066206858));
#14729=CARTESIAN_POINT('Ctrl Pts',(-6.74144616414175,-3.15244848100526,
4.77515909292762));
#14730=CARTESIAN_POINT('Ctrl Pts',(-6.93695568199013,-3.40771771847224,
4.81948145060093));
#14731=CARTESIAN_POINT('Ctrl Pts',(-7.0612422585727,-3.65351693325439,4.85745144448918));
#14732=CARTESIAN_POINT('Ctrl Pts',(-7.12604182038968,-3.99601069408371,
4.90487277263035));
#14733=CARTESIAN_POINT('Ctrl Pts',(-7.04819184769871,-4.40634676177701,
4.96169841481296));
#14734=CARTESIAN_POINT('Ctrl Pts',(-6.82636338655034,-4.7595056581786,5.01843153953646));
#14735=CARTESIAN_POINT('Ctrl Pts',(-6.49141297662963,-5.00640905746698,
5.07505897358501));
#14736=CARTESIAN_POINT('Ctrl Pts',(-6.09003751265709,-5.11411564108699,
5.13157085139478));
#14737=CARTESIAN_POINT('Ctrl Pts',(-5.6786123610455,-5.06726795065735,5.18795255071755));
#14738=CARTESIAN_POINT('Ctrl Pts',(-5.19017784555553,-4.81065089568624,
5.26294089870735));
#14739=CARTESIAN_POINT('Ctrl Pts',(-4.82877811722237,-4.18554821878284,
5.35628168565881));
#14740=CARTESIAN_POINT('Ctrl Pts',(-5.02211102820349,-3.34365258048631,
5.46759164112498));
#14741=CARTESIAN_POINT('Ctrl Pts',(-5.61197730680856,-2.94404370121664,
5.55969246505222));
#14742=CARTESIAN_POINT('Ctrl Pts',(-6.15048906815939,-2.9259067483885,5.63294612810208));
#14743=CARTESIAN_POINT('Ctrl Pts',(-6.57218830606153,-3.07274578152562,
5.69374353314818));
#14744=CARTESIAN_POINT('Ctrl Pts',(-6.92709063454883,-3.41928769105856,
5.76029112976678));
#14745=CARTESIAN_POINT('Ctrl Pts',(-7.08489845709846,-3.93331978001971,
5.83246177305221));
#14746=CARTESIAN_POINT('Ctrl Pts',(-6.97874255257226,-4.45701817474228,
5.90419082425952));
#14747=CARTESIAN_POINT('Ctrl Pts',(-6.6370356483897,-4.86355317377098,5.97546640233217));
#14748=CARTESIAN_POINT('Ctrl Pts',(-6.14579379656497,-5.05583391995401,
6.04627654027298));
#14749=CARTESIAN_POINT('Ctrl Pts',(-5.66925806099251,-4.99574215938401,
6.11075463056163));
#14750=CARTESIAN_POINT('Ctrl Pts',(-5.30691358174171,-4.76738235557255,
6.16902301258706));
#14751=CARTESIAN_POINT('Ctrl Pts',(-5.07930374249635,-4.45896349323313,
6.22119003887878));
#14752=CARTESIAN_POINT('Ctrl Pts',(-4.98082787805456,-4.09041784989305,
6.27308969220691));
#14753=CARTESIAN_POINT('Ctrl Pts',(-5.02349370691767,-3.71343965346201,
6.32471516558109));
#14754=CARTESIAN_POINT('Ctrl Pts',(-5.19999589872533,-3.37988542205928,
6.37606954207135));
#14755=CARTESIAN_POINT('Ctrl Pts',(-5.4847190912962,-3.13506427885037,6.42715348187171));
#14756=CARTESIAN_POINT('Ctrl Pts',(-5.83712621660341,-3.0121129912794,6.47796762234093));
#14757=CARTESIAN_POINT('Ctrl Pts',(-6.27051160587467,-3.0279850218392,6.5369435841435));
#14758=CARTESIAN_POINT('Ctrl Pts',(-6.71024506901487,-3.27130871222068,
6.60389475094362));
#14759=CARTESIAN_POINT('Ctrl Pts',(-6.98152291497359,-3.76371935754976,
6.67866321017483));
#14760=CARTESIAN_POINT('Ctrl Pts',(-6.95486940879079,-4.22678212803274,
6.74048184962521));
#14761=CARTESIAN_POINT('Ctrl Pts',(-6.78948845599291,-4.54563000849764,
6.78967337641285));
#14762=CARTESIAN_POINT('Ctrl Pts',(-6.58510503627771,-4.76139122419511,
6.8305173230869));
#14763=CARTESIAN_POINT('Ctrl Pts',(-6.18838065951204,-4.9729390553884,6.89153120571427));
#14764=CARTESIAN_POINT('Ctrl Pts',(-5.62852018163667,-4.92995885771748,
6.96424197979925));
#14765=CARTESIAN_POINT('Ctrl Pts',(-5.17930783991499,-4.52600430891302,
7.04445740123371));
#14766=CARTESIAN_POINT('Ctrl Pts',(-5.03049950675028,-4.00877291192731,
7.11621441643227));
#14767=CARTESIAN_POINT('Ctrl Pts',(-5.17961059739332,-3.49350571771481,
7.18758887136104));
#14768=CARTESIAN_POINT('Ctrl Pts',(-5.5773967358305,-3.13848926372906,7.25859618540072));
#14769=CARTESIAN_POINT('Ctrl Pts',(-6.10099673495183,-3.04979857717247,
7.32929304288679));
#14770=CARTESIAN_POINT('Ctrl Pts',(-6.58960034264882,-3.25249531366017,
7.39971414359334));
#14771=CARTESIAN_POINT('Ctrl Pts',(-6.89439488886565,-3.68259555007305,
7.46990161363075));
#14772=CARTESIAN_POINT('Ctrl Pts',(-6.92396663908848,-4.20760343729457,
7.53990591827929));
#14773=CARTESIAN_POINT('Ctrl Pts',(-6.66987225902436,-4.66687625782422,
7.60978068427827));
#14774=CARTESIAN_POINT('Ctrl Pts',(-6.21120047280729,-4.92032117302824,
7.67955308981974));
#14775=CARTESIAN_POINT('Ctrl Pts',(-5.68827856526509,-4.89095372189668,
7.74927925590553));
#14776=CARTESIAN_POINT('Ctrl Pts',(-5.26116058145738,-4.58792216788294,
7.81900282194838));
#14777=CARTESIAN_POINT('Ctrl Pts',(-5.0605146593326,-4.10382413158063,7.88877252132617));
#14778=CARTESIAN_POINT('Ctrl Pts',(-5.14832880834495,-3.58641746420325,
7.95863563783962));
#14779=CARTESIAN_POINT('Ctrl Pts',(-5.4984805112338,-3.19437254567264,8.02863688255444));
#14780=CARTESIAN_POINT('Ctrl Pts',(-6.0052116702054,-3.04798055828712,8.0988270789877));
#14781=CARTESIAN_POINT('Ctrl Pts',(-6.42855758612144,-3.16989299743707,
8.157498520417));
#14782=CARTESIAN_POINT('Ctrl Pts',(-6.69060506939908,-3.39192119413063,
8.20457536102132));
#14783=CARTESIAN_POINT('Ctrl Pts',(-6.87145241436045,-3.66176710955656,
8.24912648972436));
#14784=CARTESIAN_POINT('Ctrl Pts',(-6.9514390685762,-4.05527304704089,8.3030252977758));
#14785=CARTESIAN_POINT('Ctrl Pts',(-6.81226797661705,-4.50642896669386,
8.36639194934761));
#14786=CARTESIAN_POINT('Ctrl Pts',(-6.50137930109524,-4.81024489059206,
8.42475645360788));
#14787=CARTESIAN_POINT('Ctrl Pts',(-6.13147656542686,-4.93949375675132,
8.47805505000841));
#14788=CARTESIAN_POINT('Ctrl Pts',(-5.77783068564499,-4.92652168690223,
8.52621767484705));
#14789=CARTESIAN_POINT('Ctrl Pts',(-5.45197894534714,-4.78441519364883,
8.57458210426088));
#14790=CARTESIAN_POINT('Ctrl Pts',(-5.19943128109014,-4.53209841719623,
8.62316022836638));
#14791=CARTESIAN_POINT('Ctrl Pts',(-5.05584618525974,-4.20342880803269,
8.67195949129532));
#14792=CARTESIAN_POINT('Ctrl Pts',(-5.0422195366231,-3.84336351760004,8.72098742963023));
#14793=CARTESIAN_POINT('Ctrl Pts',(-5.16161137131951,-3.50154334879679,
8.77025177567099));
#14794=CARTESIAN_POINT('Ctrl Pts',(-5.39880490887244,-3.22561437898706,
8.81975828650979));
#14795=CARTESIAN_POINT('Ctrl Pts',(-5.72207914137123,-3.0546917552152,8.86951421619689));
#14796=CARTESIAN_POINT('Ctrl Pts',(-6.0872826786708,-3.01323072582504,8.91952319375617));
#14797=CARTESIAN_POINT('Ctrl Pts',(-6.444171507933,-3.10879395998011,8.96979185738356));
#14798=CARTESIAN_POINT('Ctrl Pts',(-6.74316713391831,-3.32908221727823,
9.02032286064399));
#14799=CARTESIAN_POINT('Ctrl Pts',(-6.94195230903849,-3.64511372710529,
9.07112086549811));
#14800=CARTESIAN_POINT('Ctrl Pts',(-7.01188601899995,-4.01392043220011,
9.12218639739436));
#14801=CARTESIAN_POINT('Ctrl Pts',(-6.94188943238603,-4.38461275011884,
9.17352468267902));
#14802=CARTESIAN_POINT('Ctrl Pts',(-6.71796764795472,-4.74180761880858,
9.23086676189624));
#14803=CARTESIAN_POINT('Ctrl Pts',(-6.32116660117755,-4.99875906667686,
9.29433422971609));
#14804=CARTESIAN_POINT('Ctrl Pts',(-5.80312100835904,-5.03811965025314,
9.36405136146833));
#14805=CARTESIAN_POINT('Ctrl Pts',(-5.30620047712063,-4.81454497903491,
9.43716931975444));
#14806=CARTESIAN_POINT('Ctrl Pts',(-4.97256942281115,-4.34579120199984,
9.5137592164803));
#14807=CARTESIAN_POINT('Ctrl Pts',(-4.93824840557943,-3.74461517188174,
9.59388490173077));
#14808=CARTESIAN_POINT('Ctrl Pts',(-5.23101010346705,-3.21365234345909,
9.67458646502851));
#14809=CARTESIAN_POINT('Ctrl Pts',(-5.76512274029881,-2.91777353632368,
9.75584554845314));
#14810=CARTESIAN_POINT('Ctrl Pts',(-6.37878312558969,-2.95168218807001,
9.83764095651353));
#14811=CARTESIAN_POINT('Ctrl Pts',(-6.88347692466996,-3.30911988689978,
9.91994818811354));
#14812=CARTESIAN_POINT('Ctrl Pts',(-7.12200435419038,-3.88366471751155,
10.0027398139742));
#14813=CARTESIAN_POINT('Ctrl Pts',(-7.01769174064254,-4.50040748652788,
10.0859855046625));
#14814=CARTESIAN_POINT('Ctrl Pts',(-6.5991026993888,-4.96945704213636,10.169652290447));
#14815=CARTESIAN_POINT('Ctrl Pts',(-5.99232847824897,-5.1446733592202,10.2537046806626));
#14816=CARTESIAN_POINT('Ctrl Pts',(-5.38283617149629,-4.96944471106765,
10.3381049457805));
#14817=CARTESIAN_POINT('Ctrl Pts',(-4.95848481508745,-4.49504806095511,
10.4228131773276));
#14818=CARTESIAN_POINT('Ctrl Pts',(-4.8512788133084,-3.86561185150167,10.5077878601832));
#14819=CARTESIAN_POINT('Ctrl Pts',(-5.09608303885727,-3.27408372793879,
10.5929853993213));
#14820=CARTESIAN_POINT('Ctrl Pts',(-5.61918598804022,-2.90272072154196,
10.6783618529632));
#14821=CARTESIAN_POINT('Ctrl Pts',(-6.26073803477781,-2.86658451987938,
10.7638698864798));
#14822=CARTESIAN_POINT('Ctrl Pts',(-6.82364327171669,-3.17764136170321,
10.8494663844497));
#14823=CARTESIAN_POINT('Ctrl Pts',(-7.13510597544169,-3.74083024574666,
10.9350962162971));
#14824=CARTESIAN_POINT('Ctrl Pts',(-7.09866726626603,-4.38320012653105,
11.0207290118911));
#14825=CARTESIAN_POINT('Ctrl Pts',(-6.72669125253576,-4.90762068704384,
11.1063111389501));
#14826=CARTESIAN_POINT('Ctrl Pts',(-6.13326093944664,-5.15321134684636,
11.1917885105552));
#14827=CARTESIAN_POINT('Ctrl Pts',(-5.5013182622223,-5.04585546444371,11.2771193767864));
#14828=CARTESIAN_POINT('Ctrl Pts',(-5.02452852733205,-4.61907390049617,
11.3622555821127));
#14829=CARTESIAN_POINT('Ctrl Pts',(-4.90711056796053,-4.21115651674335,
11.418857178779));
#14830=CARTESIAN_POINT('Ctrl Pts',(-4.90708301903907,-4.00651587433727,
11.447108175978));
#14831=CARTESIAN_POINT('Ctrl Pts',(-5.08958607327854,-3.99025782069458,
2.62934359726276));
#14832=CARTESIAN_POINT('Ctrl Pts',(-5.08960914627408,-3.81886565729437,
2.65300458397722));
#14833=CARTESIAN_POINT('Ctrl Pts',(-5.18775153299826,-3.47775231609314,
2.7003346517846));
#14834=CARTESIAN_POINT('Ctrl Pts',(-5.58803684598741,-3.11888353323257,
2.7718727663756));
#14835=CARTESIAN_POINT('Ctrl Pts',(-6.12129671315563,-3.02800055422244,
2.84387347131519));
#14836=CARTESIAN_POINT('Ctrl Pts',(-6.62498248189243,-3.23595716996215,
2.91641667550846));
#14837=CARTESIAN_POINT('Ctrl Pts',(-6.94329777941309,-3.68358881678574,
2.98951223929353));
#14838=CARTESIAN_POINT('Ctrl Pts',(-6.97483521943357,-4.23620018431934,
3.06319720344227));
#14839=CARTESIAN_POINT('Ctrl Pts',(-6.70566884665487,-4.72517502848787,
3.1374886735177));
#14840=CARTESIAN_POINT('Ctrl Pts',(-6.21320237967697,-4.99797593923465,
3.21240612526695));
#14841=CARTESIAN_POINT('Ctrl Pts',(-5.64636519782345,-4.96685768166421,
3.2879709618681));
#14842=CARTESIAN_POINT('Ctrl Pts',(-5.17888022725475,-4.6360306218548,3.36419310338532));
#14843=CARTESIAN_POINT('Ctrl Pts',(-4.95716603405221,-4.10260937681186,
3.44108212136025));
#14844=CARTESIAN_POINT('Ctrl Pts',(-5.05405766973863,-3.52801963757597,
3.51864211602294));
#14845=CARTESIAN_POINT('Ctrl Pts',(-5.44517562575364,-3.08929222903721,
3.5968739500623));
#14846=CARTESIAN_POINT('Ctrl Pts',(-6.01455473415458,-2.92453883772137,
3.67577419882147));
#14847=CARTESIAN_POINT('Ctrl Pts',(-6.58914066161724,-3.08930935334757,
3.75533567052421));
#14848=CARTESIAN_POINT('Ctrl Pts',(-6.97620465280587,-3.52165786554518,
3.83257632941237));
#14849=CARTESIAN_POINT('Ctrl Pts',(-7.06897925767441,-3.98066369790426,
3.89542955206584));
#14850=CARTESIAN_POINT('Ctrl Pts',(-7.01555893785241,-4.28254638624748,
3.93754537488261));
#14851=CARTESIAN_POINT('Ctrl Pts',(-6.95380842309345,-4.44582557552005,
3.96167160920718));
#14852=CARTESIAN_POINT('Ctrl Pts',(-6.83138672806294,-4.67780803645936,
3.99792061909243));
#14853=CARTESIAN_POINT('Ctrl Pts',(-6.5405370816015,-4.96217677817398,4.05251763409128));
#14854=CARTESIAN_POINT('Ctrl Pts',(-6.01531361240091,-5.11036494912871,
4.12576710362128));
#14855=CARTESIAN_POINT('Ctrl Pts',(-5.4798800948455,-4.98866772052924,4.19945314026379));
#14856=CARTESIAN_POINT('Ctrl Pts',(-5.10054865270113,-4.65370030513798,
4.26738027014));
#14857=CARTESIAN_POINT('Ctrl Pts',(-4.91834401520502,-4.2357863815548,4.32941472283313));
#14858=CARTESIAN_POINT('Ctrl Pts',(-4.90256885516074,-3.82420304826326,
4.38545643863725));
#14859=CARTESIAN_POINT('Ctrl Pts',(-5.03918037927126,-3.43420539707711,
4.44169518681064));
#14860=CARTESIAN_POINT('Ctrl Pts',(-5.33930525072368,-3.08446885471147,
4.50439031777555));
#14861=CARTESIAN_POINT('Ctrl Pts',(-5.80913211214926,-2.87223115930889,
4.57360189356491));
#14862=CARTESIAN_POINT('Ctrl Pts',(-6.37229427413888,-2.91422476933027,
4.64938345030258));
#14863=CARTESIAN_POINT('Ctrl Pts',(-6.74888177129849,-3.15750352412239,
4.709582128297));
#14864=CARTESIAN_POINT('Ctrl Pts',(-6.94490140998246,-3.41339882099762,
4.75401894510768));
#14865=CARTESIAN_POINT('Ctrl Pts',(-7.06970558341153,-3.66017127708851,
4.79214595145499));
#14866=CARTESIAN_POINT('Ctrl Pts',(-7.13500723247069,-4.00480166501556,
4.83987187277834));
#14867=CARTESIAN_POINT('Ctrl Pts',(-7.05655517105359,-4.41899249863413,
4.89723555158439));
#14868=CARTESIAN_POINT('Ctrl Pts',(-6.83208424000845,-4.77657076660703,
4.95467781113089));
#14869=CARTESIAN_POINT('Ctrl Pts',(-6.49207156199412,-5.02736404071781,
5.0121827474206));
#14870=CARTESIAN_POINT('Ctrl Pts',(-6.08339025242798,-5.13715599402453,
5.06973475823005));
#14871=CARTESIAN_POINT('Ctrl Pts',(-5.66322179904519,-5.08942531962948,
5.12731904881901));
#14872=CARTESIAN_POINT('Ctrl Pts',(-5.16297094376659,-4.82679185368301,
5.2041196620197));
#14873=CARTESIAN_POINT('Ctrl Pts',(-4.79066213150166,-4.18431414464998,
5.3001343861563));
#14874=CARTESIAN_POINT('Ctrl Pts',(-4.98965381173811,-3.31366183574818,
5.4152322895872));
#14875=CARTESIAN_POINT('Ctrl Pts',(-5.60225840489793,-2.89783757391139,
5.51095527979351));
#14876=CARTESIAN_POINT('Ctrl Pts',(-6.16385669310836,-2.87878317991021,
5.58735141171596));
#14877=CARTESIAN_POINT('Ctrl Pts',(-6.60462995607195,-3.03216488094667,
5.65090073233228));
#14878=CARTESIAN_POINT('Ctrl Pts',(-6.97665349261024,-3.39515151898213,
5.72063857301452));
#14879=CARTESIAN_POINT('Ctrl Pts',(-7.14265993135726,-3.93521632088349,
5.79647782910357));
#14880=CARTESIAN_POINT('Ctrl Pts',(-7.0310083056303,-4.4869108207016,5.87203948693374));
#14881=CARTESIAN_POINT('Ctrl Pts',(-6.67033948104626,-4.91626585048744,
5.94730014972142));
#14882=CARTESIAN_POINT('Ctrl Pts',(-6.15060695231922,-5.11985532484333,
6.02222597416855));
#14883=CARTESIAN_POINT('Ctrl Pts',(-5.64541150540802,-5.05627265809946,
6.09058083970922));
#14884=CARTESIAN_POINT('Ctrl Pts',(-5.26069476946472,-4.81388570953019,
6.15244175228014));
#14885=CARTESIAN_POINT('Ctrl Pts',(-5.01875583364388,-4.4861215358841,6.20788483808207));
#14886=CARTESIAN_POINT('Ctrl Pts',(-4.9139522084251,-4.09406610320522,6.26309574236783));
#14887=CARTESIAN_POINT('Ctrl Pts',(-4.95934334049254,-3.69270060694395,
6.31805861073807));
#14888=CARTESIAN_POINT('Ctrl Pts',(-5.14735742783483,-3.33732783794384,
6.37276806703712));
#14889=CARTESIAN_POINT('Ctrl Pts',(-5.45082896178906,-3.07635399284825,
6.42721536466454));
#14890=CARTESIAN_POINT('Ctrl Pts',(-5.82657935181436,-2.94524248695214,
6.48139347544157));
#14891=CARTESIAN_POINT('Ctrl Pts',(-6.28875793296553,-2.96214980134559,
6.54428133364918));
#14892=CARTESIAN_POINT('Ctrl Pts',(-6.7577138250312,-3.221654892675,6.61568080479831));
#14893=CARTESIAN_POINT('Ctrl Pts',(-7.046869499807,-3.74657137930345,6.69536653730686));
#14894=CARTESIAN_POINT('Ctrl Pts',(-7.01842122365346,-4.23984048730701,
6.76121511684626));
#14895=CARTESIAN_POINT('Ctrl Pts',(-6.84239266572927,-4.57917463164239,
6.81356230981021));
#14896=CARTESIAN_POINT('Ctrl Pts',(-6.62501763362136,-4.8086423485827,6.85699845424774));
#14897=CARTESIAN_POINT('Ctrl Pts',(-6.20340460181096,-5.03340444241976,
6.921826051713));
#14898=CARTESIAN_POINT('Ctrl Pts',(-5.60959457936301,-4.98752605922673,
6.99894677554392));
#14899=CARTESIAN_POINT('Ctrl Pts',(-5.13461428204011,-4.56008255639909,
7.08377299672669));
#14900=CARTESIAN_POINT('Ctrl Pts',(-4.9778500212962,-4.01441171084717,7.15945663213478));
#14901=CARTESIAN_POINT('Ctrl Pts',(-5.13490417096659,-3.4726580148424,7.23449301164271));
#14902=CARTESIAN_POINT('Ctrl Pts',(-5.55195715900246,-3.10081935662606,
7.30889700246225));
#14903=CARTESIAN_POINT('Ctrl Pts',(-6.09863068969014,-3.00854209579386,
7.3826886113079));
#14904=CARTESIAN_POINT('Ctrl Pts',(-6.60648447138017,-3.21958594141858,
7.45589041854474));
#14905=CARTESIAN_POINT('Ctrl Pts',(-6.9216791982701,-3.66497931973675,7.52852965123266));
#14906=CARTESIAN_POINT('Ctrl Pts',(-6.95177924004462,-4.20587447720696,
7.60063489875532));
#14907=CARTESIAN_POINT('Ctrl Pts',(-6.6909662386489,-4.67646854269574,7.67223803710999));
#14908=CARTESIAN_POINT('Ctrl Pts',(-6.22299726037103,-4.93459747092674,
7.7433777926895));
#14909=CARTESIAN_POINT('Ctrl Pts',(-5.69254032107038,-4.90439315263447,
7.81409150036152));
#14910=CARTESIAN_POINT('Ctrl Pts',(-5.2618365955028,-4.59831452234616,7.88442076722058));
#14911=CARTESIAN_POINT('Ctrl Pts',(-5.06089011399604,-4.11241503492589,
7.95440897609695));
#14912=CARTESIAN_POINT('Ctrl Pts',(-5.14891476057707,-3.5962099799928,8.02410112276677));
#14913=CARTESIAN_POINT('Ctrl Pts',(-5.49666377882435,-3.20746270201702,
8.09354551735423));
#14914=CARTESIAN_POINT('Ctrl Pts',(-5.99681265084705,-3.06340348104051,
8.16278786553222));
#14915=CARTESIAN_POINT('Ctrl Pts',(-6.41224590200003,-3.18336826033736,
8.22037117887724));
#14916=CARTESIAN_POINT('Ctrl Pts',(-6.66836775683141,-3.40046253258805,
8.26638619207942));
#14917=CARTESIAN_POINT('Ctrl Pts',(-6.84466758932173,-3.66362380044245,
8.30982365803551));
#14918=CARTESIAN_POINT('Ctrl Pts',(-6.92216235674791,-4.04596600254198,
8.36217057302082));
#14919=CARTESIAN_POINT('Ctrl Pts',(-6.78729405069043,-4.48230953614279,
8.42346277729895));
#14920=CARTESIAN_POINT('Ctrl Pts',(-6.48766998582839,-4.77482452426569,
8.47967703069394));
#14921=CARTESIAN_POINT('Ctrl Pts',(-6.13255927907409,-4.8987822245107,8.53083176826075));
#14922=CARTESIAN_POINT('Ctrl Pts',(-5.79405373663887,-4.88627598976337,
8.57692529241349));
#14923=CARTESIAN_POINT('Ctrl Pts',(-5.48301690867117,-4.7505320540268,8.62309299030759));
#14924=CARTESIAN_POINT('Ctrl Pts',(-5.24260511121906,-4.51022473960559,
8.6693420733107));
#14925=CARTESIAN_POINT('Ctrl Pts',(-5.10628760740664,-4.19799093789299,
8.71569057208715));
#14926=CARTESIAN_POINT('Ctrl Pts',(-5.09344745751731,-3.85672818834445,
8.76215292714239));
#14927=CARTESIAN_POINT('Ctrl Pts',(-5.2064383924313,-3.53345566112826,8.80874199058791));
#14928=CARTESIAN_POINT('Ctrl Pts',(-5.43040665899872,-3.27300345792075,
8.85547704096572));
#14929=CARTESIAN_POINT('Ctrl Pts',(-5.73509299001327,-3.11197616335786,
8.90236484872161));
#14930=CARTESIAN_POINT('Ctrl Pts',(-6.07874463617352,-3.07301201788798,
8.94941993516621));
#14931=CARTESIAN_POINT('Ctrl Pts',(-6.41409907073854,-3.16285967160041,
8.9966547034903));
#14932=CARTESIAN_POINT('Ctrl Pts',(-6.69471463191465,-3.36965539654581,
9.04408229994015));
#14933=CARTESIAN_POINT('Ctrl Pts',(-6.88108384841174,-3.66601330952044,
9.09171381385298));
#14934=CARTESIAN_POINT('Ctrl Pts',(-6.9465780164732,-4.01156860735228,9.13955827692911));
#14935=CARTESIAN_POINT('Ctrl Pts',(-6.88101508718794,-4.35867292221011,
9.18763006950063));
#14936=CARTESIAN_POINT('Ctrl Pts',(-6.67141125514706,-4.6929894095024,9.24130109606731));
#14937=CARTESIAN_POINT('Ctrl Pts',(-6.30010945166128,-4.93341342253205,
9.300689301377));
#14938=CARTESIAN_POINT('Ctrl Pts',(-5.81536145282493,-4.97024504354847,
9.36592731075453));
#14939=CARTESIAN_POINT('Ctrl Pts',(-5.35021909987976,-4.76099072350817,
9.43437195900332));
#14940=CARTESIAN_POINT('Ctrl Pts',(-5.03767451365318,-4.32196228839712,
9.50611541884564));
#14941=CARTESIAN_POINT('Ctrl Pts',(-5.00539919271839,-3.7582617467778,9.58125324423978));
#14942=CARTESIAN_POINT('Ctrl Pts',(-5.28020380225241,-3.25961343195422,
9.65704139684407));
#14943=CARTESIAN_POINT('Ctrl Pts',(-5.78257562978636,-2.98114555664001,
9.73349075256426));
#14944=CARTESIAN_POINT('Ctrl Pts',(-6.36108530515163,-3.012933580896,9.81060861195967));
#14945=CARTESIAN_POINT('Ctrl Pts',(-6.83813479497314,-3.35054278443211,
9.8883982005671));
#14946=CARTESIAN_POINT('Ctrl Pts',(-7.06436526891603,-3.89486967330545,
9.9668588526319));
#14947=CARTESIAN_POINT('Ctrl Pts',(-6.9654778242667,-4.48105551001564,10.0459859100048));
#14948=CARTESIAN_POINT('Ctrl Pts',(-6.5665776770944,-4.92845750971493,10.1257707953368));
#14949=CARTESIAN_POINT('Ctrl Pts',(-5.9861285159527,-5.09638198019228,10.2062010449906));
#14950=CARTESIAN_POINT('Ctrl Pts',(-5.40077430176762,-4.92842380855109,
10.2872603721036));
#14951=CARTESIAN_POINT('Ctrl Pts',(-4.99147369823858,-4.47135751604514,
10.3689288026212));
#14952=CARTESIAN_POINT('Ctrl Pts',(-4.88737185959524,-3.86224827783339,
10.4511826978566));
#14953=CARTESIAN_POINT('Ctrl Pts',(-5.12493606869768,-3.2872555983534,10.5339951511892));
#14954=CARTESIAN_POINT('Ctrl Pts',(-5.6352408565221,-2.92451464581263,10.6173355355939));
#14955=CARTESIAN_POINT('Ctrl Pts',(-6.2640751739065,-2.88870996291299,10.7011710889467));
#14956=CARTESIAN_POINT('Ctrl Pts',(-6.81848291382748,-3.19462273696641,
10.7854640234358));
#14957=CARTESIAN_POINT('Ctrl Pts',(-7.12686484968034,-3.75143580561001,
10.870178671056));
#14958=CARTESIAN_POINT('Ctrl Pts',(-7.09106689040093,-4.38964946962175,
10.9552663097424));
#14959=CARTESIAN_POINT('Ctrl Pts',(-6.72015560018353,-4.91323638810909,
11.0406886438574));
#14960=CARTESIAN_POINT('Ctrl Pts',(-6.12535013441635,-5.15984551571332,
11.1263955783573));
#14961=CARTESIAN_POINT('Ctrl Pts',(-5.4888177159,-5.05207984615036,11.2123531394243));
#14962=CARTESIAN_POINT('Ctrl Pts',(-5.00618128684596,-4.62072035504479,
11.2984791152375));
#14963=CARTESIAN_POINT('Ctrl Pts',(-4.88655223846457,-4.20611915635318,
11.3560320854752));
#14964=CARTESIAN_POINT('Ctrl Pts',(-4.88652420961371,-3.9979134719832,11.3847752429281));
#14965=CARTESIAN_POINT('Ctrl Pts',(-5.11146388820137,-4.00349311292524,
2.72519423144341));
#14966=CARTESIAN_POINT('Ctrl Pts',(-5.1114863896228,-3.83634674945349,2.74826907808176));
#14967=CARTESIAN_POINT('Ctrl Pts',(-5.2073386709242,-3.50459135808253,2.79432654428865));
#14968=CARTESIAN_POINT('Ctrl Pts',(-5.59392162451954,-3.15886603128654,
2.86334120921819));
#14969=CARTESIAN_POINT('Ctrl Pts',(-6.10462882761145,-3.07233116043825,
2.93229890548955));
#14970=CARTESIAN_POINT('Ctrl Pts',(-6.58324742293624,-3.27049009618399,
3.00126508671495));
#14971=CARTESIAN_POINT('Ctrl Pts',(-6.88338780506893,-3.69336482148996,
3.07028562510752));
#14972=CARTESIAN_POINT('Ctrl Pts',(-6.9125378234219,-4.21176138753265,3.13941249417303));
#14973=CARTESIAN_POINT('Ctrl Pts',(-6.66117842543386,-4.66753315377219,
3.20869846013298));
#14974=CARTESIAN_POINT('Ctrl Pts',(-6.20426035603016,-4.92022504844555,
3.27819713364705));
#14975=CARTESIAN_POINT('Ctrl Pts',(-5.68113059624983,-4.89117330402607,
3.34794822940351));
#14976=CARTESIAN_POINT('Ctrl Pts',(-5.25170796397958,-4.58692564876463,
3.41800289998785));
#14977=CARTESIAN_POINT('Ctrl Pts',(-5.04895699031254,-4.09847602344442,
3.48840459466937));
#14978=CARTESIAN_POINT('Ctrl Pts',(-5.13758843731787,-3.57411477941281,
3.5591972982065));
#14979=CARTESIAN_POINT('Ctrl Pts',(-5.49375906320309,-3.17483235058257,
3.63042148845005));
#14980=CARTESIAN_POINT('Ctrl Pts',(-6.01112620351243,-3.02524985044883,
3.7021155619589));
#14981=CARTESIAN_POINT('Ctrl Pts',(-6.53249037329618,-3.17483138875088,
3.77431501475635));
#14982=CARTESIAN_POINT('Ctrl Pts',(-6.88345308070225,-3.56688559200541,
3.84435825865076));
#14983=CARTESIAN_POINT('Ctrl Pts',(-6.96758670253936,-3.98305434767195,
3.90134832783096));
#14984=CARTESIAN_POINT('Ctrl Pts',(-6.91914662613188,-4.25684126103168,
3.93954468754766));
#14985=CARTESIAN_POINT('Ctrl Pts',(-6.86313250970625,-4.40495668933761,
3.96143027230283));
#14986=CARTESIAN_POINT('Ctrl Pts',(-6.75206286997603,-4.61543115327382,
3.99431845667718));
#14987=CARTESIAN_POINT('Ctrl Pts',(-6.48808491278166,-4.8736085272702,4.04387852104861));
#14988=CARTESIAN_POINT('Ctrl Pts',(-6.01074296926441,-5.00838471988809,
4.11045312998563));
#14989=CARTESIAN_POINT('Ctrl Pts',(-5.52325638980643,-4.89771417726584,
4.17753632489081));
#14990=CARTESIAN_POINT('Ctrl Pts',(-5.17709404353748,-4.59222957518482,
4.23950256233906));
#14991=CARTESIAN_POINT('Ctrl Pts',(-5.01043388242926,-4.21016874273666,
4.29621843833516));
#14992=CARTESIAN_POINT('Ctrl Pts',(-4.99589713399363,-3.83310074843265,
4.34755840879351));
#14993=CARTESIAN_POINT('Ctrl Pts',(-5.12125994677539,-3.47495912195723,
4.39919681737111));
#14994=CARTESIAN_POINT('Ctrl Pts',(-5.39743127754854,-3.15296659074283,
4.45690341966157));
#14995=CARTESIAN_POINT('Ctrl Pts',(-5.83115129685322,-2.95679680521155,
4.52080615558924));
#14996=CARTESIAN_POINT('Ctrl Pts',(-6.35316218281195,-2.99545324585569,
4.5910453945408));
#14997=CARTESIAN_POINT('Ctrl Pts',(-6.70376257092702,-3.22166688646999,
4.64705710233426));
#14998=CARTESIAN_POINT('Ctrl Pts',(-6.88678372913165,-3.46054900968793,
4.68853934391483));
#14999=CARTESIAN_POINT('Ctrl Pts',(-7.0035074423105,-3.69129846575723,4.72419072967401));
#15000=CARTESIAN_POINT('Ctrl Pts',(-7.06484203667896,-4.01438157828431,
4.76893210034011));
#15001=CARTESIAN_POINT('Ctrl Pts',(-6.99115886817154,-4.40411780678025,
4.82290082050557));
#15002=CARTESIAN_POINT('Ctrl Pts',(-6.77930308964722,-4.74188330839879,
4.87714191961237));
#15003=CARTESIAN_POINT('Ctrl Pts',(-6.45705491738398,-4.97974523614269,
4.93165021696835));
#15004=CARTESIAN_POINT('Ctrl Pts',(-6.06815028839713,-5.08439258892097,
4.98641872200361));
#15005=CARTESIAN_POINT('Ctrl Pts',(-5.66662034905994,-5.03892039260337,
5.04143952880628));
#15006=CARTESIAN_POINT('Ctrl Pts',(-5.18655285081867,-4.78714708110153,
5.11512653518091));
#15007=CARTESIAN_POINT('Ctrl Pts',(-4.82613499448797,-4.16740651020841,
5.20781216493432));
#15008=CARTESIAN_POINT('Ctrl Pts',(-5.01848603257964,-3.31910069175158,
5.31989761553554));
#15009=CARTESIAN_POINT('Ctrl Pts',(-5.61981332624524,-2.9094932624567,5.41393698760798));
#15010=CARTESIAN_POINT('Ctrl Pts',(-6.17547145334383,-2.89038655816394,
5.48950913679716));
#15011=CARTESIAN_POINT('Ctrl Pts',(-6.61354799505512,-3.04263063984369,
5.55265712784929));
#15012=CARTESIAN_POINT('Ctrl Pts',(-6.98549988101616,-3.40498346435387,
5.62232050138183));
#15013=CARTESIAN_POINT('Ctrl Pts',(-7.15276763293528,-3.94768190565954,
5.69853201897246));
#15014=CARTESIAN_POINT('Ctrl Pts',(-7.04028187626715,-4.50564202791614,
5.77493404150203));
#15015=CARTESIAN_POINT('Ctrl Pts',(-6.67370872730767,-4.94268691087855,
5.8514836989803));
#15016=CARTESIAN_POINT('Ctrl Pts',(-6.14199125879717,-5.15141832358651,
5.92815184332714));
#15017=CARTESIAN_POINT('Ctrl Pts',(-5.62193267759359,-5.08634477712989,
5.99850052868461));
#15018=CARTESIAN_POINT('Ctrl Pts',(-5.22382985790438,-4.83573996048168,
6.06248404381697));
#15019=CARTESIAN_POINT('Ctrl Pts',(-4.97233041446878,-4.49530252943299,
6.12008460662565));
#15020=CARTESIAN_POINT('Ctrl Pts',(-4.86283729649089,-4.08632133851381,
6.17767307025924));
#15021=CARTESIAN_POINT('Ctrl Pts',(-4.91023011228302,-3.66584228236825,
6.2352433234891));
#15022=CARTESIAN_POINT('Ctrl Pts',(-5.10784440922835,-3.29200270232238,
6.29277619099215));
#15023=CARTESIAN_POINT('Ctrl Pts',(-5.42817465514537,-3.01632843786686,
6.35025789696987));
#15024=CARTESIAN_POINT('Ctrl Pts',(-5.82638908712853,-2.87723611583061,
6.40767362354461));
#15025=CARTESIAN_POINT('Ctrl Pts',(-6.31803709458161,-2.89504436194142,
6.47456205294508));
#15026=CARTESIAN_POINT('Ctrl Pts',(-6.81932677366183,-3.17198486831857,
6.55085313024292));
#15027=CARTESIAN_POINT('Ctrl Pts',(-7.13022853870334,-3.73544410660141,
6.63640199512977));
#15028=CARTESIAN_POINT('Ctrl Pts',(-7.09985484999904,-4.26766588322049,
6.70744516442597));
#15029=CARTESIAN_POINT('Ctrl Pts',(-6.90937626959466,-4.63499910749687,
6.7640986891494));
#15030=CARTESIAN_POINT('Ctrl Pts',(-6.67363197611175,-4.88389416051919,
6.81120623918702));
#15031=CARTESIAN_POINT('Ctrl Pts',(-6.21540678092779,-5.1283578591014,6.88167501898689));
#15032=CARTESIAN_POINT('Ctrl Pts',(-5.56750905972414,-5.07878760962261,
6.96581377607078));
#15033=CARTESIAN_POINT('Ctrl Pts',(-5.04725897731621,-4.61100994769211,
7.05867824449733));
#15034=CARTESIAN_POINT('Ctrl Pts',(-4.87502236930835,-4.01211284223512,
7.14174757031646));
#15035=CARTESIAN_POINT('Ctrl Pts',(-5.04762190701414,-3.41622257144757,
7.22427184785083));
#15036=CARTESIAN_POINT('Ctrl Pts',(-5.50694650780015,-3.00656473703432,
7.3062269716042));
#15037=CARTESIAN_POINT('Ctrl Pts',(-6.10967519422246,-2.90477651653003,
7.38758405539665));
#15038=CARTESIAN_POINT('Ctrl Pts',(-6.66982264240046,-3.13755152778926,
7.46832293040742));
#15039=CARTESIAN_POINT('Ctrl Pts',(-7.01735971004567,-3.62873051387297,
7.54842470644817));
#15040=CARTESIAN_POINT('Ctrl Pts',(-7.05042704618396,-4.22472296521213,
7.62787559478529));
#15041=CARTESIAN_POINT('Ctrl Pts',(-6.76331769359956,-4.74244592149819,
7.70666504495723));
#15042=CARTESIAN_POINT('Ctrl Pts',(-6.24935597182185,-5.02571530571555,
7.78478624180885));
#15043=CARTESIAN_POINT('Ctrl Pts',(-5.66841983881672,-4.992387139032,7.86223669086622));
#15044=CARTESIAN_POINT('Ctrl Pts',(-5.19841826828567,-4.65801741457885,
7.93901781676939));
#15045=CARTESIAN_POINT('Ctrl Pts',(-4.98021276748805,-4.12948856160228,
8.0151347855238));
#15046=CARTESIAN_POINT('Ctrl Pts',(-5.07589799354624,-3.57067831525686,
8.09059738471413));
#15047=CARTESIAN_POINT('Ctrl Pts',(-5.45083661313803,-3.1521641999378,8.1654177239109));
#15048=CARTESIAN_POINT('Ctrl Pts',(-5.98682154391905,-2.99827751934189,
8.23961543820677));
#15049=CARTESIAN_POINT('Ctrl Pts',(-6.42909049947727,-3.12640964775913,
8.30093785873061));
#15050=CARTESIAN_POINT('Ctrl Pts',(-6.70043358144534,-3.35653176806574,
8.3497078062489));
#15051=CARTESIAN_POINT('Ctrl Pts',(-6.88657968867636,-3.63453023876189,
8.39558817150443));
#15052=CARTESIAN_POINT('Ctrl Pts',(-6.96771103676148,-4.03652906886562,
8.45063175096959));
#15053=CARTESIAN_POINT('Ctrl Pts',(-6.82648710559109,-4.49210420145525,
8.51464865041861));
#15054=CARTESIAN_POINT('Ctrl Pts',(-6.51539277681862,-4.79529496351186,
8.57297461574563));
#15055=CARTESIAN_POINT('Ctrl Pts',(-6.14916965403812,-4.92292264363337,
8.62573226691127));
#15056=CARTESIAN_POINT('Ctrl Pts',(-5.80196913848439,-4.909917389324,8.67302067136497));
#15057=CARTESIAN_POINT('Ctrl Pts',(-5.48474830529899,-4.77128250666151,
8.72012180414365));
#15058=CARTESIAN_POINT('Ctrl Pts',(-5.24095336372299,-4.52733379926624,
8.76705651381845));
#15059=CARTESIAN_POINT('Ctrl Pts',(-5.10357198259525,-4.21220488751096,
8.81383360157659));
#15060=CARTESIAN_POINT('Ctrl Pts',(-5.09086860733029,-3.8697568592241,8.86046614728715));
#15061=CARTESIAN_POINT('Ctrl Pts',(-5.20379231374995,-3.54721450725183,
8.90696898921786));
#15062=CARTESIAN_POINT('Ctrl Pts',(-5.42617914586712,-3.28888235937374,
8.95334950953911));
#15063=CARTESIAN_POINT('Ctrl Pts',(-5.72694661343973,-3.13011803590362,
8.99962946343878));
#15064=CARTESIAN_POINT('Ctrl Pts',(-6.06427021742266,-3.09205710176064,
9.04582166245532));
#15065=CARTESIAN_POINT('Ctrl Pts',(-6.39160236864643,-3.17992456672212,
9.09194056693847));
#15066=CARTESIAN_POINT('Ctrl Pts',(-6.66398918720521,-3.38086998734912,
9.13799988910989));
#15067=CARTESIAN_POINT('Ctrl Pts',(-6.84387671595628,-3.66722063438552,
9.18401494103932));
#15068=CARTESIAN_POINT('Ctrl Pts',(-6.9066670679967,-3.9993466547744,9.23000347197484));
#15069=CARTESIAN_POINT('Ctrl Pts',(-6.84382580193358,-4.33123468360912,
9.27597545458883));
#15070=CARTESIAN_POINT('Ctrl Pts',(-6.64420674116633,-4.6493173671815,9.32706132906817));
#15071=CARTESIAN_POINT('Ctrl Pts',(-6.29259770566886,-4.87662537775517,
9.38327712956274));
#15072=CARTESIAN_POINT('Ctrl Pts',(-5.83643195943725,-4.91096143644274,
9.44467383294874));
#15073=CARTESIAN_POINT('Ctrl Pts',(-5.40126345522019,-4.71485427181151,
9.50873917863421));
#15074=CARTESIAN_POINT('Ctrl Pts',(-5.11067191095492,-4.3060141160397,9.57552502373875));
#15075=CARTESIAN_POINT('Ctrl Pts',(-5.08114749160738,-3.78409491879455,
9.64510336845023));
#15076=CARTESIAN_POINT('Ctrl Pts',(-5.33465759113435,-3.32474188581643,
9.71495303907397));
#15077=CARTESIAN_POINT('Ctrl Pts',(-5.79582326317987,-3.06943273025373,
9.78512080947981));
#15078=CARTESIAN_POINT('Ctrl Pts',(-6.32483990648236,-3.09873681028405,
9.85565111386688));
#15079=CARTESIAN_POINT('Ctrl Pts',(-6.75970042212355,-3.40672284706517,
9.92658636274972));
#15080=CARTESIAN_POINT('Ctrl Pts',(-6.96536307562826,-3.90194183503021,
9.99796648875838));
#15081=CARTESIAN_POINT('Ctrl Pts',(-6.87546272288741,-4.43425542219748,
10.0698288137258));
#15082=CARTESIAN_POINT('Ctrl Pts',(-6.51357040107586,-4.84006961009873,
10.1422077693513));
#15083=CARTESIAN_POINT('Ctrl Pts',(-5.987291243916,-4.99231483046356,10.215134731367));
#15084=CARTESIAN_POINT('Ctrl Pts',(-5.45650767309877,-4.84005420013297,
10.2886378275285));
#15085=CARTESIAN_POINT('Ctrl Pts',(-5.08506221166951,-4.42538406867581,
10.3627417782245));
#15086=CARTESIAN_POINT('Ctrl Pts',(-4.990363336042,-3.87204197816745,10.4374677368732));
#15087=CARTESIAN_POINT('Ctrl Pts',(-5.20641176001674,-3.34868167362847,
10.5128331669689));
#15088=CARTESIAN_POINT('Ctrl Pts',(-5.67177590318358,-3.01762544047152,
10.5888517859959));
#15089=CARTESIAN_POINT('Ctrl Pts',(-6.24696780354825,-2.98461711370722,
10.6655333487327));
#15090=CARTESIAN_POINT('Ctrl Pts',(-6.75588576872762,-3.26509285809973,
10.7428838921771));
#15091=CARTESIAN_POINT('Ctrl Pts',(-7.04023081280776,-3.777787551644,10.8209050268513));
#15092=CARTESIAN_POINT('Ctrl Pts',(-7.00749304795215,-4.36808121544397,
10.8995954448141));
#15093=CARTESIAN_POINT('Ctrl Pts',(-6.66323831848384,-4.85473674137387,
10.9789522846304));
#15094=CARTESIAN_POINT('Ctrl Pts',(-6.10814274891664,-5.08536413962976,
11.0589563184805));
#15095=CARTESIAN_POINT('Ctrl Pts',(-5.51078426858185,-4.98467662470909,
11.1396132151697));
#15096=CARTESIAN_POINT('Ctrl Pts',(-5.05510117731205,-4.57809092709479,
11.2208625878388));
#15097=CARTESIAN_POINT('Ctrl Pts',(-4.94130014896063,-4.18467098041075,
11.275481957862));
#15098=CARTESIAN_POINT('Ctrl Pts',(-4.94127348351102,-3.98659299949179,
11.3028269682096));
#15099=CARTESIAN_POINT('Ctrl Pts',(-5.04970734608444,-4.014134093399,2.80233410707682));
#15100=CARTESIAN_POINT('Ctrl Pts',(-5.04973134605583,-3.83585611419469,
2.82694569265781));
#15101=CARTESIAN_POINT('Ctrl Pts',(-5.15206923445116,-3.4823776986807,2.8760204246601));
#15102=CARTESIAN_POINT('Ctrl Pts',(-5.5614206316956,-3.1170823820106,2.9490162429901));
#15103=CARTESIAN_POINT('Ctrl Pts',(-6.09810765925963,-3.02662690392752,
3.02147152025646));
#15104=CARTESIAN_POINT('Ctrl Pts',(-6.59712262306125,-3.23386828229798,
3.09339820603842));
#15105=CARTESIAN_POINT('Ctrl Pts',(-6.90732475729933,-3.67194259316541,
3.1648380955771));
#15106=CARTESIAN_POINT('Ctrl Pts',(-6.93665430754779,-4.20438646265423,
3.23582612292702));
#15107=CARTESIAN_POINT('Ctrl Pts',(-6.68004065809059,-4.6684075873074,3.30640045570415));
#15108=CARTESIAN_POINT('Ctrl Pts',(-6.21810008921364,-4.92314954604884,
3.37659939052329));
#15109=CARTESIAN_POINT('Ctrl Pts',(-5.69397648524808,-4.8934201192585,3.4464749107676));
#15110=CARTESIAN_POINT('Ctrl Pts',(-5.26764630093375,-4.59059929678225,
3.51606935423513));
#15111=CARTESIAN_POINT('Ctrl Pts',(-5.06841388342893,-4.10903719737237,
3.58543200219124));
#15112=CARTESIAN_POINT('Ctrl Pts',(-5.15562823873306,-3.59663109925005,
3.65461124945938));
#15113=CARTESIAN_POINT('Ctrl Pts',(-5.50139878391617,-3.20987562699863,
3.72365749828155));
#15114=CARTESIAN_POINT('Ctrl Pts',(-5.99930358470049,-3.0664980755698,3.79262171549619));
#15115=CARTESIAN_POINT('Ctrl Pts',(-6.49701819772681,-3.20984963236153,
3.86155496989464));
#15116=CARTESIAN_POINT('Ctrl Pts',(-6.82941314564483,-3.58189551733825,
3.92795571781378));
#15117=CARTESIAN_POINT('Ctrl Pts',(-6.90838988314061,-3.97403261720178,
3.98163963232954));
#15118=CARTESIAN_POINT('Ctrl Pts',(-6.86289779162592,-4.23089029905683,
4.01747350728414));
#15119=CARTESIAN_POINT('Ctrl Pts',(-6.81044462585338,-4.36957346598223,
4.03796496216898));
#15120=CARTESIAN_POINT('Ctrl Pts',(-6.70657469009075,-4.56638426544445,
4.06871708209625));
#15121=CARTESIAN_POINT('Ctrl Pts',(-6.46041372675795,-4.80683684920928,
4.11489392405871));
#15122=CARTESIAN_POINT('Ctrl Pts',(-6.01759168782143,-4.93159391025523,
4.17664209312006));
#15123=CARTESIAN_POINT('Ctrl Pts',(-5.56748440020554,-4.82915336507103,
4.23858440378004));
#15124=CARTESIAN_POINT('Ctrl Pts',(-5.24923420310336,-4.54803781304708,
4.29557297658576));
#15125=CARTESIAN_POINT('Ctrl Pts',(-5.09649486695971,-4.19765775733976,
4.34757880141343));
#15126=CARTESIAN_POINT('Ctrl Pts',(-5.08327146603833,-3.8527045728546,4.39454228313687));
#15127=CARTESIAN_POINT('Ctrl Pts',(-5.19778067898822,-3.5257764501926,4.4416810635407));
#15128=CARTESIAN_POINT('Ctrl Pts',(-5.44949654344042,-3.23240173071767,
4.49426376054938));
#15129=CARTESIAN_POINT('Ctrl Pts',(-5.84405907648008,-3.05405527712975,
4.5523889489519));
#15130=CARTESIAN_POINT('Ctrl Pts',(-6.31813331118975,-3.0892458106026,4.61617835220101));
#15131=CARTESIAN_POINT('Ctrl Pts',(-6.63615534979497,-3.2945021411286,4.66698598908312));
#15132=CARTESIAN_POINT('Ctrl Pts',(-6.80211652576663,-3.51112312284911,
4.70460183160974));
#15133=CARTESIAN_POINT('Ctrl Pts',(-6.90794042502969,-3.72033578077783,
4.73692473637605));
#15134=CARTESIAN_POINT('Ctrl Pts',(-6.96353651155719,-4.01321756900286,
4.77748340064075));
#15135=CARTESIAN_POINT('Ctrl Pts',(-6.8967395362674,-4.36654451491255,4.82640965537421));
#15136=CARTESIAN_POINT('Ctrl Pts',(-6.70462301696789,-4.67285941150863,
4.87559975444018));
#15137=CARTESIAN_POINT('Ctrl Pts',(-6.41222708309043,-4.88870995426925,
4.9250602957143));
#15138=CARTESIAN_POINT('Ctrl Pts',(-6.05905690187772,-4.98377296921959,
4.97479876152583));
#15139=CARTESIAN_POINT('Ctrl Pts',(-5.69401310371,-4.94246805059484,5.02481952450994));
#15140=CARTESIAN_POINT('Ctrl Pts',(-5.25700058678662,-4.71334498855493,
5.09189738429313));
#15141=CARTESIAN_POINT('Ctrl Pts',(-4.92782438010502,-4.14811605570046,
5.17646870468282));
#15142=CARTESIAN_POINT('Ctrl Pts',(-5.10336010603255,-3.37095253982733,
5.27914266109507));
#15143=CARTESIAN_POINT('Ctrl Pts',(-5.65645834162634,-2.99345132990119,
5.36570023443787));
#15144=CARTESIAN_POINT('Ctrl Pts',(-6.1699913664732,-2.97563873503376,5.43554293217881));
#15145=CARTESIAN_POINT('Ctrl Pts',(-6.57603542854649,-3.11664200174749,
5.49407461937123));
#15146=CARTESIAN_POINT('Ctrl Pts',(-6.92218952721961,-3.4535052357566,5.55887865709695));
#15147=CARTESIAN_POINT('Ctrl Pts',(-7.07875034877777,-3.96045691179561,
5.63008959061315));
#15148=CARTESIAN_POINT('Ctrl Pts',(-6.97347642065377,-4.48421269602345,
5.70180458156708));
#15149=CARTESIAN_POINT('Ctrl Pts',(-6.62798627215935,-4.89664122684824,
5.774012746944));
#15150=CARTESIAN_POINT('Ctrl Pts',(-6.12405454097509,-5.09484079360517,
5.84669765808443));
#15151=CARTESIAN_POINT('Ctrl Pts',(-5.62839476656752,-5.03315023883122,
5.91374936242762));
#15152=CARTESIAN_POINT('Ctrl Pts',(-5.24707290574412,-4.79332552679213,
5.97502813879928));
#15153=CARTESIAN_POINT('Ctrl Pts',(-5.00513094556786,-4.46608144539262,
6.0304158049875));
#15154=CARTESIAN_POINT('Ctrl Pts',(-4.89923307934873,-4.07118717667332,
6.08603667815864));
#15155=CARTESIAN_POINT('Ctrl Pts',(-4.94503254732023,-3.66338243335723,
6.14187603551199));
#15156=CARTESIAN_POINT('Ctrl Pts',(-5.13737019634667,-3.2991604706762,6.19792514865836));
#15157=CARTESIAN_POINT('Ctrl Pts',(-5.45065975015127,-3.02931466187735,
6.25417235306358));
#15158=CARTESIAN_POINT('Ctrl Pts',(-5.84195458942871,-2.89246212692768,
6.31060529244871));
#15159=CARTESIAN_POINT('Ctrl Pts',(-6.32729017217876,-2.90982944532215,
6.37664874935649));
#15160=CARTESIAN_POINT('Ctrl Pts',(-6.82518249543237,-3.18428897290923,
6.45238921757374));
#15161=CARTESIAN_POINT('Ctrl Pts',(-7.13653729570471,-3.74723934336787,
6.53793129879579));
#15162=CARTESIAN_POINT('Ctrl Pts',(-7.10645173764727,-4.28288462039874,
6.60943086415581));
#15163=CARTESIAN_POINT('Ctrl Pts',(-6.91387636050383,-4.65453678643226,
6.66674636099218));
#15164=CARTESIAN_POINT('Ctrl Pts',(-6.67463855570598,-4.90719225117517,
6.7145634081676));
#15165=CARTESIAN_POINT('Ctrl Pts',(-6.20793365325718,-5.15650233906366,
6.78637308174185));
#15166=CARTESIAN_POINT('Ctrl Pts',(-5.54326866993286,-5.10667068723003,
6.8726820373125));
#15167=CARTESIAN_POINT('Ctrl Pts',(-5.00498017679516,-4.62367347193851,
6.96868726861754));
#15168=CARTESIAN_POINT('Ctrl Pts',(-4.82528676773444,-4.00081830567214,
7.05510807363504));
#15169=CARTESIAN_POINT('Ctrl Pts',(-5.0053951436861,-3.37689823861283,7.14150364401192));
#15170=CARTESIAN_POINT('Ctrl Pts',(-5.48872482401552,-2.94511360670821,
7.22781068048454));
#15171=CARTESIAN_POINT('Ctrl Pts',(-6.12700755803508,-2.83678576185677,
7.31398732955836));
#15172=CARTESIAN_POINT('Ctrl Pts',(-6.72375384707874,-3.08423079176768,
7.3999797427674));
#15173=CARTESIAN_POINT('Ctrl Pts',(-7.09619313569336,-3.60980021306789,
7.48573840517752));
#15174=CARTESIAN_POINT('Ctrl Pts',(-7.13220207582214,-4.25095033753033,
7.57121852214645));
#15175=CARTESIAN_POINT('Ctrl Pts',(-6.82226807006467,-4.8106779703119,7.65637806859443));
#15176=CARTESIAN_POINT('Ctrl Pts',(-6.26467177253605,-5.11841193742535,
7.74116325228304));
#15177=CARTESIAN_POINT('Ctrl Pts',(-5.6318275183675,-5.08243517581132,7.82553668780451));
#15178=CARTESIAN_POINT('Ctrl Pts',(-5.11797960895723,-4.71721968706553,
7.90945703925193));
#15179=CARTESIAN_POINT('Ctrl Pts',(-4.87859187879085,-4.13801197139399,
7.99288822687277));
#15180=CARTESIAN_POINT('Ctrl Pts',(-4.98352628418032,-3.52404020081029,
8.07579636929506));
#15181=CARTESIAN_POINT('Ctrl Pts',(-5.39610472469272,-3.06329341970928,
8.15814987354169));
#15182=CARTESIAN_POINT('Ctrl Pts',(-5.98679900925825,-2.89359357100788,
8.23992344671619));
#15183=CARTESIAN_POINT('Ctrl Pts',(-6.47460873131575,-3.03488339301435,
8.30755819903438));
#15184=CARTESIAN_POINT('Ctrl Pts',(-6.7739262603932,-3.2887285566142,8.361354258082));
#15185=CARTESIAN_POINT('Ctrl Pts',(-6.97925131350371,-3.59536714231701,
8.41196069057612));
#15186=CARTESIAN_POINT('Ctrl Pts',(-7.06869487572216,-4.03865184085066,
8.47265070023439));
#15187=CARTESIAN_POINT('Ctrl Pts',(-6.91302940167929,-4.5405717591675,8.54318103210321));
#15188=CARTESIAN_POINT('Ctrl Pts',(-6.57067014159411,-4.87411806202039,
8.60735327160586));
#15189=CARTESIAN_POINT('Ctrl Pts',(-6.16833388604433,-5.01426844190105,
8.66530637083758));
#15190=CARTESIAN_POINT('Ctrl Pts',(-5.78753541605273,-4.99995160631877,
8.71716535362411));
#15191=CARTESIAN_POINT('Ctrl Pts',(-5.44029859859097,-4.84812019841673,
8.76872529749127));
#15192=CARTESIAN_POINT('Ctrl Pts',(-5.17404859244767,-4.58160005133281,
8.81998703566189));
#15193=CARTESIAN_POINT('Ctrl Pts',(-5.02442632985894,-4.23818465699728,
8.87095201100959));
#15194=CARTESIAN_POINT('Ctrl Pts',(-5.01071327042434,-3.86603779547018,
8.92162223867994));
#15195=CARTESIAN_POINT('Ctrl Pts',(-5.133161597464,-3.51659961675723,8.97200070786022));
#15196=CARTESIAN_POINT('Ctrl Pts',(-5.37343817646623,-3.23765328783206,
9.02209162753279));
#15197=CARTESIAN_POINT('Ctrl Pts',(-5.69721379739349,-3.06688291613834,
9.07189898149531));
#15198=CARTESIAN_POINT('Ctrl Pts',(-6.05895785997844,-3.02618452117534,
9.12142738396272));
#15199=CARTESIAN_POINT('Ctrl Pts',(-6.40855782530253,-3.12017328225075,
9.1706837654698));
#15200=CARTESIAN_POINT('Ctrl Pts',(-6.69823038132667,-3.33403896702626,
9.21967431232278));
#15201=CARTESIAN_POINT('Ctrl Pts',(-6.88863293580495,-3.63740928685802,
9.26840700272366));
#15202=CARTESIAN_POINT('Ctrl Pts',(-6.95467920020127,-3.98761029148836,
9.3168884619293));
#15203=CARTESIAN_POINT('Ctrl Pts',(-6.88857999906526,-4.33587510882518,
9.365129823227));
#15204=CARTESIAN_POINT('Ctrl Pts',(-6.67995054872608,-4.66795372110108,
9.41847144777411));
#15205=CARTESIAN_POINT('Ctrl Pts',(-6.31469728103988,-4.9036483621764,9.47683205548445));
#15206=CARTESIAN_POINT('Ctrl Pts',(-5.84433052501836,-4.93863276025009,
9.54012573212548));
#15207=CARTESIAN_POINT('Ctrl Pts',(-5.39902615361661,-4.73746267851064,
9.6056963980877));
#15208=CARTESIAN_POINT('Ctrl Pts',(-5.10430163036973,-4.32178849006536,
9.67352801570003));
#15209=CARTESIAN_POINT('Ctrl Pts',(-5.075187070932,-3.79592840074772,9.74361293322054));
#15210=CARTESIAN_POINT('Ctrl Pts',(-5.32901434535869,-3.33728385728079,
9.81338743259124));
#15211=CARTESIAN_POINT('Ctrl Pts',(-5.78624334014352,-3.08485820545814,
9.88289796408472));
#15212=CARTESIAN_POINT('Ctrl Pts',(-6.30604928044245,-3.11425799421081,
9.95219289498374));
#15213=CARTESIAN_POINT('Ctrl Pts',(-6.72956367609471,-3.41493193430552,
10.021321716681));
#15214=CARTESIAN_POINT('Ctrl Pts',(-6.92790783320255,-3.89402420811448,
10.0903350063486));
#15215=CARTESIAN_POINT('Ctrl Pts',(-6.84109464889487,-4.40474031567081,
10.1592840124265));
#15216=CARTESIAN_POINT('Ctrl Pts',(-6.49597320364271,-4.79095463264426,
10.2282203670656));
#15217=CARTESIAN_POINT('Ctrl Pts',(-5.99800616609963,-4.93448878448542,
10.2971957723242));
#15218=CARTESIAN_POINT('Ctrl Pts',(-5.49933195557159,-4.79095105026251,
10.3662617164922));
#15219=CARTESIAN_POINT('Ctrl Pts',(-5.1527139367811,-4.40334569175967,10.4354691299253));
#15220=CARTESIAN_POINT('Ctrl Pts',(-5.06514889324528,-3.8893268520199,10.5048681455515));
#15221=CARTESIAN_POINT('Ctrl Pts',(-5.26513463485952,-3.40581804738845,
10.5745075879262));
#15222=CARTESIAN_POINT('Ctrl Pts',(-5.69343493256485,-3.10151979632748,
10.6444352547726));
#15223=CARTESIAN_POINT('Ctrl Pts',(-6.22052717215153,-3.07154871751346,
10.7146962814146));
#15224=CARTESIAN_POINT('Ctrl Pts',(-6.68521110233421,-3.32791229650645,
10.7853358376373));
#15225=CARTESIAN_POINT('Ctrl Pts',(-6.9440279852268,-3.7949758640772,10.8563922071995));
#15226=CARTESIAN_POINT('Ctrl Pts',(-6.91413085988338,-4.33148339801506,
10.927911347834));
#15227=CARTESIAN_POINT('Ctrl Pts',(-6.60162688016772,-4.77309716981846,
10.9999287290131));
#15228=CARTESIAN_POINT('Ctrl Pts',(-6.09828367789878,-4.9821600137055,11.0724702098908));
#15229=CARTESIAN_POINT('Ctrl Pts',(-5.55679798821165,-4.89091465998753,
11.1455776779411));
#15230=CARTESIAN_POINT('Ctrl Pts',(-5.14358275601793,-4.5222302433581,11.2192552432817));
#15231=CARTESIAN_POINT('Ctrl Pts',(-5.04025189628822,-4.16531630046125,
11.2688069686638));
#15232=CARTESIAN_POINT('Ctrl Pts',(-5.04022766416365,-3.9853136985979,11.2936566414427));
#15233=CARTESIAN_POINT('Ctrl Pts',(-4.95040444753908,-4.01407741549073,
2.80202038668682));
#15234=CARTESIAN_POINT('Ctrl Pts',(-4.95043088631308,-3.81768338133247,
2.82913292521151));
#15235=CARTESIAN_POINT('Ctrl Pts',(-5.06328046757572,-3.42769328904537,
2.88327944150245));
#15236=CARTESIAN_POINT('Ctrl Pts',(-5.51483986880678,-3.02481655682361,
2.96379357401038));
#15237=CARTESIAN_POINT('Ctrl Pts',(-6.10663155887047,-2.92510416783479,
3.04369524283156));
#15238=CARTESIAN_POINT('Ctrl Pts',(-6.65627932676067,-3.15350765201444,
3.12292801020133));
#15239=CARTESIAN_POINT('Ctrl Pts',(-6.9972996120088,-3.63538358706421,3.20150185546868));
#15240=CARTESIAN_POINT('Ctrl Pts',(-7.02927375427223,-4.21966673835877,
3.27940299578842));
#15241=CARTESIAN_POINT('Ctrl Pts',(-6.7482428987564,-4.72729484195001,3.35663488008679));
#15242=CARTESIAN_POINT('Ctrl Pts',(-6.24433772797396,-5.00482166130207,
3.43319919431017));
#15243=CARTESIAN_POINT('Ctrl Pts',(-5.67509809740256,-4.97217848865363,
3.50910146535417));
#15244=CARTESIAN_POINT('Ctrl Pts',(-5.21440956091332,-4.64446921121479,
3.58435286234765));
#15245=CARTESIAN_POINT('Ctrl Pts',(-5.00052648608049,-4.12635602119185,
3.65896760418264));
#15246=CARTESIAN_POINT('Ctrl Pts',(-5.09426410583311,-3.57844077526578,
3.73296399244798));
#15247=CARTESIAN_POINT('Ctrl Pts',(-5.46214956932136,-3.16771217138052,
3.80636392097382));
#15248=CARTESIAN_POINT('Ctrl Pts',(-5.98800389280316,-3.01684552839974,
3.87919268136819));
#15249=CARTESIAN_POINT('Ctrl Pts',(-6.50966711131542,-3.16768533912665,
3.95147944874766));
#15250=CARTESIAN_POINT('Ctrl Pts',(-6.85516841335202,-3.55524247398461,
4.02059719986475));
#15251=CARTESIAN_POINT('Ctrl Pts',(-6.93640504947824,-3.96044008918348,
4.07607464042623));
#15252=CARTESIAN_POINT('Ctrl Pts',(-6.88959590680744,-4.22437715215301,
4.11290351758767));
#15253=CARTESIAN_POINT('Ctrl Pts',(-6.83583101050569,-4.36650480320736,
4.13390569410839));
#15254=CARTESIAN_POINT('Ctrl Pts',(-6.7295526054213,-4.5678453422278,4.16536800412348));
#15255=CARTESIAN_POINT('Ctrl Pts',(-6.4785719176604,-4.81253370237805,4.21242247700862));
#15256=CARTESIAN_POINT('Ctrl Pts',(-6.03075890744692,-4.93824024016166,
4.27485498317197));
#15257=CARTESIAN_POINT('Ctrl Pts',(-5.57912503362765,-4.83500621126696,
4.33703045129724));
#15258=CARTESIAN_POINT('Ctrl Pts',(-5.26234982431842,-4.55465959483225,
4.39381979062297));
#15259=CARTESIAN_POINT('Ctrl Pts',(-5.11135697875295,-4.20781103939821,
4.44529674263384));
#15260=CARTESIAN_POINT('Ctrl Pts',(-5.09852187023819,-3.86824490814822,
4.49153434459407));
#15261=CARTESIAN_POINT('Ctrl Pts',(-5.21076926661952,-3.54825343245558,
4.53768901317022));
#15262=CARTESIAN_POINT('Ctrl Pts',(-5.4560334473407,-3.26270136286835,4.5888995411409));
#15263=CARTESIAN_POINT('Ctrl Pts',(-5.83799792334387,-3.09044094457653,
4.64515534859482));
#15264=CARTESIAN_POINT('Ctrl Pts',(-6.29359570267334,-3.12464990354928,
4.70646757272288));
#15265=CARTESIAN_POINT('Ctrl Pts',(-6.5971317711187,-3.32088855862012,4.75500854197238));
#15266=CARTESIAN_POINT('Ctrl Pts',(-6.75487078461784,-3.52682180277232,
4.79077023674625));
#15267=CARTESIAN_POINT('Ctrl Pts',(-6.85522021528563,-3.72525753530104,
4.82142962589092));
#15268=CARTESIAN_POINT('Ctrl Pts',(-6.90765078845783,-4.00210628009459,
4.85976988485919));
#15269=CARTESIAN_POINT('Ctrl Pts',(-6.84466700781614,-4.33458160329838,
4.90581898898127));
#15270=CARTESIAN_POINT('Ctrl Pts',(-6.66451131395465,-4.62157482642531,
4.95192414686361));
#15271=CARTESIAN_POINT('Ctrl Pts',(-6.39151660574891,-4.82296908084052,
4.99809965612829));
#15272=CARTESIAN_POINT('Ctrl Pts',(-6.06305555872298,-4.91125610532342,
5.04435858184245));
#15273=CARTESIAN_POINT('Ctrl Pts',(-5.72479607824289,-4.87288998099965,
5.09071672932403));
#15274=CARTESIAN_POINT('Ctrl Pts',(-5.32120053858948,-4.66111598189267,
5.15267699940499));
#15275=CARTESIAN_POINT('Ctrl Pts',(-5.01901830093614,-4.14106232858579,
5.2304571964414));
#15276=CARTESIAN_POINT('Ctrl Pts',(-5.18022338687198,-3.43017789857566,
5.32440560742871));
#15277=CARTESIAN_POINT('Ctrl Pts',(-5.6844669484819,-3.08645264353291,5.40329988483335));
#15278=CARTESIAN_POINT('Ctrl Pts',(-6.15144238874992,-3.07029944892001,
5.46681719664217));
#15279=CARTESIAN_POINT('Ctrl Pts',(-6.52026173698852,-3.19841233327777,
5.51998619154465));
#15280=CARTESIAN_POINT('Ctrl Pts',(-6.83432988576568,-3.50411755194789,
5.57879302796362));
#15281=CARTESIAN_POINT('Ctrl Pts',(-6.97628146059944,-3.96381837777065,
5.64337000548355));
#15282=CARTESIAN_POINT('Ctrl Pts',(-6.88084694300038,-4.43864700704047,
5.70838686985743));
#15283=CARTESIAN_POINT('Ctrl Pts',(-6.56758301987762,-4.81266288881362,
5.77386709056138));
#15284=CARTESIAN_POINT('Ctrl Pts',(-6.11031818471074,-4.99257534235218,
5.83982471574392));
#15285=CARTESIAN_POINT('Ctrl Pts',(-5.66001412277134,-4.93661451797503,
5.90073884439067));
#15286=CARTESIAN_POINT('Ctrl Pts',(-5.31308429830285,-4.71849225798761,
5.95648421056427));
#15287=CARTESIAN_POINT('Ctrl Pts',(-5.09263031894632,-4.42040358314247,
6.00694184124335));
#15288=CARTESIAN_POINT('Ctrl Pts',(-4.99593329451219,-4.06008832376263,
6.05769248289879));
#15289=CARTESIAN_POINT('Ctrl Pts',(-5.03772761005556,-3.68727382498282,
6.10873703661228));
#15290=CARTESIAN_POINT('Ctrl Pts',(-5.21384768597732,-3.35358843624591,
6.1600783267073));
#15291=CARTESIAN_POINT('Ctrl Pts',(-5.5014279300585,-3.10576378920885,6.21171698888381));
#15292=CARTESIAN_POINT('Ctrl Pts',(-5.86154480647318,-2.97971897775594,
6.26365397549107));
#15293=CARTESIAN_POINT('Ctrl Pts',(-6.30941327345328,-2.99561470365393,
6.32459355700482));
#15294=CARTESIAN_POINT('Ctrl Pts',(-6.77065800699938,-3.24951148750743,
6.39473524121105));
#15295=CARTESIAN_POINT('Ctrl Pts',(-7.0607018985248,-3.77301027291914,6.47429880651946));
#15296=CARTESIAN_POINT('Ctrl Pts',(-7.03292138795243,-4.27386006447141,
6.54114742255594));
#15297=CARTESIAN_POINT('Ctrl Pts',(-6.85223599948128,-4.62277890659896,
6.59494154091868));
#15298=CARTESIAN_POINT('Ctrl Pts',(-6.62708269893594,-4.86061413836101,
6.63994414492635));
#15299=CARTESIAN_POINT('Ctrl Pts',(-6.18654127549617,-5.09621068018119,
6.70774704639851));
#15300=CARTESIAN_POINT('Ctrl Pts',(-5.55521460528796,-5.04973111393953,
6.78971417043737));
#15301=CARTESIAN_POINT('Ctrl Pts',(-5.03992134796692,-4.5883040965929,6.88151516750169));
#15302=CARTESIAN_POINT('Ctrl Pts',(-4.86647072351276,-3.98899998152023,
6.96467750538145));
#15303=CARTESIAN_POINT('Ctrl Pts',(-5.04035634712671,-3.3845330871616,7.04834093198449));
#15304=CARTESIAN_POINT('Ctrl Pts',(-5.51120006351292,-2.96311388418359,
7.13247929982247));
#15305=CARTESIAN_POINT('Ctrl Pts',(-6.13755247913796,-2.85620971181115,
7.21704708882013));
#15306=CARTESIAN_POINT('Ctrl Pts',(-6.72743904042145,-3.10014807205115,
7.30200621015969));
#15307=CARTESIAN_POINT('Ctrl Pts',(-7.09845727328089,-3.62266975603267,
7.38731447687665));
#15308=CARTESIAN_POINT('Ctrl Pts',(-7.13514378651329,-4.26482661359482,
7.47292307371327));
#15309=CARTESIAN_POINT('Ctrl Pts',(-6.82312421498377,-4.82958152399516,
7.55878062096553));
#15310=CARTESIAN_POINT('Ctrl Pts',(-6.25727921934041,-5.14256327876596,
7.64484924170431));
#15311=CARTESIAN_POINT('Ctrl Pts',(-5.61038110386298,-5.10639049644132,
7.73107411010418));
#15312=CARTESIAN_POINT('Ctrl Pts',(-5.0813191910786,-4.73109282931615,7.81740648211959));
#15313=CARTESIAN_POINT('Ctrl Pts',(-4.83286177762465,-4.13147349319584,
7.90379432673586));
#15314=CARTESIAN_POINT('Ctrl Pts',(-4.94165930199982,-3.4914906721837,7.99018552170849));
#15315=CARTESIAN_POINT('Ctrl Pts',(-5.3738945619569,-3.00797620488942,8.07652992915658));
#15316=CARTESIAN_POINT('Ctrl Pts',(-5.99684003484179,-2.82845004799815,
8.1627717509804));
#15317=CARTESIAN_POINT('Ctrl Pts',(-6.51449684023436,-2.97795530901467,
8.23452455634887));
#15318=CARTESIAN_POINT('Ctrl Pts',(-6.83340937345703,-3.24831236496221,
8.29182387018181));
#15319=CARTESIAN_POINT('Ctrl Pts',(-7.05275944220763,-3.57577124194805,
8.3458718722718));
#15320=CARTESIAN_POINT('Ctrl Pts',(-7.14888836510883,-4.05081892701449,
8.41090607558749));
#15321=CARTESIAN_POINT('Ctrl Pts',(-6.98158887614932,-4.59121631424625,
8.48682539302922));
#15322=CARTESIAN_POINT('Ctrl Pts',(-6.6117457325826,-4.95188043527737,8.55617619977002));
#15323=CARTESIAN_POINT('Ctrl Pts',(-6.17552481242006,-5.10395058079544,
8.61900798734293));
#15324=CARTESIAN_POINT('Ctrl Pts',(-5.76155504078242,-5.08847730642841,
8.6753791908211));
#15325=CARTESIAN_POINT('Ctrl Pts',(-5.3831114419134,-4.92309348031777,8.73156508207711));
#15326=CARTESIAN_POINT('Ctrl Pts',(-5.09226942582765,-4.63206374041745,
8.78754752252364));
#15327=CARTESIAN_POINT('Ctrl Pts',(-4.92846639521676,-4.25626808792367,
8.84331833042908));
#15328=CARTESIAN_POINT('Ctrl Pts',(-4.91337499340381,-3.84826985979358,
8.89886725533888));
#15329=CARTESIAN_POINT('Ctrl Pts',(-5.04778839460805,-3.46454521355224,
8.95418338540694));
#15330=CARTESIAN_POINT('Ctrl Pts',(-5.31195836233809,-3.15779237445369,
9.00926172959177));
#15331=CARTESIAN_POINT('Ctrl Pts',(-5.66836068440024,-2.96977926794819,
9.06408851803747));
#15332=CARTESIAN_POINT('Ctrl Pts',(-6.0669191210522,-2.92491551484476,9.11865767650999));
#15333=CARTESIAN_POINT('Ctrl Pts',(-6.45235041531044,-3.02852547184126,
9.17296094526983));
#15334=CARTESIAN_POINT('Ctrl Pts',(-6.77183369988165,-3.26439524326313,
9.2269931450209));
#15335=CARTESIAN_POINT('Ctrl Pts',(-6.98185220328006,-3.59902874792769,
9.28074746802313));
#15336=CARTESIAN_POINT('Ctrl Pts',(-7.05467848322916,-3.98526890769635,
9.33421836644156));
#15337=CARTESIAN_POINT('Ctrl Pts',(-6.98178576790913,-4.36920823973671,
9.38740267928406));
#15338=CARTESIAN_POINT('Ctrl Pts',(-6.75190034469451,-4.73504959901346,
9.44617221538153));
#15339=CARTESIAN_POINT('Ctrl Pts',(-6.34988721691645,-4.99435744148628,
9.51039990537655));
#15340=CARTESIAN_POINT('Ctrl Pts',(-5.833124943149,-5.03265791293926,9.57993884000276));
#15341=CARTESIAN_POINT('Ctrl Pts',(-5.34505445198339,-4.81197730828659,
9.6518236665488));
#15342=CARTESIAN_POINT('Ctrl Pts',(-5.02312104102536,-4.35746827773343,
9.72597446942884));
#15343=CARTESIAN_POINT('Ctrl Pts',(-4.99173885665344,-3.78474783904724,
9.80231093424411));
#15344=CARTESIAN_POINT('Ctrl Pts',(-5.26733037366742,-3.28753608995048,
9.87798912154192));
#15345=CARTESIAN_POINT('Ctrl Pts',(-5.7610100142267,-3.01545532543433,9.95302085463951));
#15346=CARTESIAN_POINT('Ctrl Pts',(-6.31901312620276,-3.04746542801833,
10.0274218227863));
#15347=CARTESIAN_POINT('Ctrl Pts',(-6.77073258958868,-3.36875755220951,
10.1012114179017));
#15348=CARTESIAN_POINT('Ctrl Pts',(-6.98060223215716,-3.87703875799955,
10.1744126613645));
#15349=CARTESIAN_POINT('Ctrl Pts',(-6.88862190599467,-4.41490833473546,
10.2470520646821));
#15350=CARTESIAN_POINT('Ctrl Pts',(-6.52726603979659,-4.81843912722608,
10.3191594492329));
#15351=CARTESIAN_POINT('Ctrl Pts',(-6.01022364648023,-4.96686190627768,
10.390767804212));
#15352=CARTESIAN_POINT('Ctrl Pts',(-5.49680133015996,-4.81845446474053,
10.4619130490713));
#15353=CARTESIAN_POINT('Ctrl Pts',(-5.14312970083041,-4.42204619402635,
10.5326339259449));
#15354=CARTESIAN_POINT('Ctrl Pts',(-5.05500684830352,-3.90108130763402,
10.6029715447986));
#15355=CARTESIAN_POINT('Ctrl Pts',(-5.25654917398459,-3.41542914409823,
10.6729696033374));
#15356=CARTESIAN_POINT('Ctrl Pts',(-5.68373908537632,-3.11267812572593,
10.7426732040747));
#15357=CARTESIAN_POINT('Ctrl Pts',(-6.20470547300614,-3.08367627152615,
10.8121306435434));
#15358=CARTESIAN_POINT('Ctrl Pts',(-6.6599080173046,-3.33549556127491,10.8813885520368));
#15359=CARTESIAN_POINT('Ctrl Pts',(-6.91104727221352,-3.78995831176175,
10.9505019065133));
#15360=CARTESIAN_POINT('Ctrl Pts',(-6.88163942109489,-4.30749866343159,
11.0195109771094));
#15361=CARTESIAN_POINT('Ctrl Pts',(-6.58197977005813,-4.73002117605488,
11.0884704057876));
#15362=CARTESIAN_POINT('Ctrl Pts',(-6.10331498315377,-4.92825339378842,
11.157438247149));
#15363=CARTESIAN_POINT('Ctrl Pts',(-5.59217136013618,-4.84169576209836,
11.2264590988613));
#15364=CARTESIAN_POINT('Ctrl Pts',(-5.20484579854406,-4.49541939104753,
11.2955951659005));
#15365=CARTESIAN_POINT('Ctrl Pts',(-5.10870499490301,-4.16277367149241,
11.3417785121125));
#15366=CARTESIAN_POINT('Ctrl Pts',(-5.10868242823946,-3.99514255262147,
11.3649202801113));
#15367=CARTESIAN_POINT('Ctrl Pts',(-4.88818719635698,-4.00347727294065,
2.72529722008525));
#15368=CARTESIAN_POINT('Ctrl Pts',(-4.8882151797164,-3.79560965978366,2.75399370617715));
#15369=CARTESIAN_POINT('Ctrl Pts',(-5.00768402952602,-3.38176479254249,
2.8114458207661));
#15370=CARTESIAN_POINT('Ctrl Pts',(-5.48912761258474,-2.95155104882261,
2.89735388716427));
#15371=CARTESIAN_POINT('Ctrl Pts',(-6.12367588859993,-2.84418536850341,
2.9830394830188));
#15372=CARTESIAN_POINT('Ctrl Pts',(-6.71608295773462,-3.08988004512223,
3.06841689939367));
#15373=CARTESIAN_POINT('Ctrl Pts',(-7.08548551208247,-3.61116247844501,
3.15345759772618));
#15374=CARTESIAN_POINT('Ctrl Pts',(-7.12058610325535,-4.24603336903534,
3.23810936636211));
#15375=CARTESIAN_POINT('Ctrl Pts',(-6.81439089049297,-4.79977673821013,
3.32233710953462));
#15376=CARTESIAN_POINT('Ctrl Pts',(-6.26324852083861,-5.10364407717512,
3.40610338036098));
#15377=CARTESIAN_POINT('Ctrl Pts',(-5.63880259300186,-5.06806358715257,
3.489365903903));
#15378=CARTESIAN_POINT('Ctrl Pts',(-5.1322299275751,-4.70793906273771,3.57209477752228));
#15379=CARTESIAN_POINT('Ctrl Pts',(-4.89657596527452,-4.13743625505341,
3.65425891220947));
#15380=CARTESIAN_POINT('Ctrl Pts',(-4.99983412380025,-3.53336895261622,
3.73583244193299));
#15381=CARTESIAN_POINT('Ctrl Pts',(-5.4056138863883,-3.08027815183281,3.81679205719959));
#15382=CARTESIAN_POINT('Ctrl Pts',(-5.98566419848572,-2.9138752058618,3.89711855437139));
#15383=CARTESIAN_POINT('Ctrl Pts',(-6.5607175758941,-3.08021552425877,3.97679599518704));
#15384=CARTESIAN_POINT('Ctrl Pts',(-6.94104043806148,-3.50699914121927,
4.05288638067068));
#15385=CARTESIAN_POINT('Ctrl Pts',(-7.03023256912709,-3.95237226486497,
4.11385241520314));
#15386=CARTESIAN_POINT('Ctrl Pts',(-6.97884494814435,-4.24201642458273,
4.15426575236254));
#15387=CARTESIAN_POINT('Ctrl Pts',(-6.91989134069545,-4.39785579457805,
4.17729322914019));
#15388=CARTESIAN_POINT('Ctrl Pts',(-6.80342892392235,-4.61848748240129,
4.21176796422099));
#15389=CARTESIAN_POINT('Ctrl Pts',(-6.52880823922492,-4.88607101119092,
4.2632233953033));
#15390=CARTESIAN_POINT('Ctrl Pts',(-6.040337156624,-5.02298743966762,4.33131125112158));
#15391=CARTESIAN_POINT('Ctrl Pts',(-5.54956390280064,-4.91056640618497,
4.39887183410603));
#15392=CARTESIAN_POINT('Ctrl Pts',(-5.20684987950378,-4.60696587191263,
4.46032308612493));
#15393=CARTESIAN_POINT('Ctrl Pts',(-5.04416577721804,-4.23292269389065,
4.51582356884532));
#15394=CARTESIAN_POINT('Ctrl Pts',(-5.03048913212015,-3.86809303813757,
4.56548891208506));
#15395=CARTESIAN_POINT('Ctrl Pts',(-5.15075591711637,-3.52565244918924,
4.61488073233877));
#15396=CARTESIAN_POINT('Ctrl Pts',(-5.41232829565927,-3.22134006592063,
4.66945984212975));
#15397=CARTESIAN_POINT('Ctrl Pts',(-5.81764466923774,-3.03889776937362,
4.72912569596472));
#15398=CARTESIAN_POINT('Ctrl Pts',(-6.29802642946598,-3.07534304184591,
4.79377063220834));
#15399=CARTESIAN_POINT('Ctrl Pts',(-6.61583128941994,-3.28116081870527,
4.84458999703416));
#15400=CARTESIAN_POINT('Ctrl Pts',(-6.78033519526549,-3.49597871671357,
4.88188763378668));
#15401=CARTESIAN_POINT('Ctrl Pts',(-6.88472108499998,-3.70245984060303,
4.91378208472349));
#15402=CARTESIAN_POINT('Ctrl Pts',(-6.93893227813884,-3.98943532436169,
4.9535135694603));
#15403=CARTESIAN_POINT('Ctrl Pts',(-6.87381560608202,-4.33220427041261,
5.00098425193981));
#15404=CARTESIAN_POINT('Ctrl Pts',(-6.68890774242002,-4.62645671922366,
5.04825821317051));
#15405=CARTESIAN_POINT('Ctrl Pts',(-6.41032716352109,-4.83174064470429,
5.09534896646907));
#15406=CARTESIAN_POINT('Ctrl Pts',(-6.07704473350618,-4.92113376655074,
5.14227039283988));
#15407=CARTESIAN_POINT('Ctrl Pts',(-5.73578768023823,-4.88225536268528,
5.1890341934005));
#15408=CARTESIAN_POINT('Ctrl Pts',(-5.33090189374131,-4.66950551714918,
5.25119580619967));
#15409=CARTESIAN_POINT('Ctrl Pts',(-5.03127344889024,-4.15143713732072,
5.32855279023866));
#15410=CARTESIAN_POINT('Ctrl Pts',(-5.19141108346178,-3.45225578202365,
5.42097872761472));
#15411=CARTESIAN_POINT('Ctrl Pts',(-5.68285225510471,-3.11865945660659,
5.49774652619562));
#15412=CARTESIAN_POINT('Ctrl Pts',(-6.13381349440763,-3.10330694154298,
5.55908224617128));
#15413=CARTESIAN_POINT('Ctrl Pts',(-6.48818012667083,-3.22657080017143,
5.61016324701949));
#15414=CARTESIAN_POINT('Ctrl Pts',(-6.78797228127654,-3.51887282825301,
5.66633206213167));
#15415=CARTESIAN_POINT('Ctrl Pts',(-6.92236393580735,-3.95532434325643,
5.72761512040668));
#15416=CARTESIAN_POINT('Ctrl Pts',(-6.83198717655826,-4.40328470381393,
5.78895467537118));
#15417=CARTESIAN_POINT('Ctrl Pts',(-6.53784519235893,-4.75395986679681,
5.85037529513985));
#15418=CARTESIAN_POINT('Ctrl Pts',(-6.11102395408416,-4.92157115925373,
5.91192019317696));
#15419=CARTESIAN_POINT('Ctrl Pts',(-5.69291374826433,-4.86935449914238,
5.96847486209515));
#15420=CARTESIAN_POINT('Ctrl Pts',(-5.37211663285,-4.66750507041932,6.02002466665042));
#15421=CARTESIAN_POINT('Ctrl Pts',(-5.16891943289149,-4.39259029914511,
6.06654729043601));
#15422=CARTESIAN_POINT('Ctrl Pts',(-5.08012035782711,-4.06130362216233,
6.11319817659068));
#15423=CARTESIAN_POINT('Ctrl Pts',(-5.118529628433,-3.71945211312213,6.1600007209651));
#15424=CARTESIAN_POINT('Ctrl Pts',(-5.27972004240338,-3.41422893411933,
6.20696368569299));
#15425=CARTESIAN_POINT('Ctrl Pts',(-5.54230107336362,-3.18804339540855,
6.25410140038552));
#15426=CARTESIAN_POINT('Ctrl Pts',(-5.87047888260951,-3.07324172255546,
6.30142586543012));
#15427=CARTESIAN_POINT('Ctrl Pts',(-6.27796878089394,-3.08777452389964,
6.3568679207874));
#15428=CARTESIAN_POINT('Ctrl Pts',(-6.69691616492966,-3.31851514648166,
6.42058411199161));
#15429=CARTESIAN_POINT('Ctrl Pts',(-6.95995510674012,-3.79348275334223,
6.4927626682328));
#15430=CARTESIAN_POINT('Ctrl Pts',(-6.93474143742393,-4.24754819527297,
6.55336750542438));
#15431=CARTESIAN_POINT('Ctrl Pts',(-6.77094422938177,-4.56384857799987,
6.60213386431775));
#15432=CARTESIAN_POINT('Ctrl Pts',(-6.56680914225599,-4.77947610755828,
6.6429345197011));
#15433=CARTESIAN_POINT('Ctrl Pts',(-6.16731733865748,-4.99313041589805,
6.70442493094763));
#15434=CARTESIAN_POINT('Ctrl Pts',(-5.59427289252952,-4.95110526236717,
6.7788227895025));
#15435=CARTESIAN_POINT('Ctrl Pts',(-5.12557736184267,-4.5316246663191,6.86231296849033));
#15436=CARTESIAN_POINT('Ctrl Pts',(-4.9673444927583,-3.98552765323417,6.93810379755276));
#15437=CARTESIAN_POINT('Ctrl Pts',(-5.12600956760141,-3.43315316105931,
7.01455793974746));
#15438=CARTESIAN_POINT('Ctrl Pts',(-5.5573775358164,-3.04671481003938,7.09167935720874));
#15439=CARTESIAN_POINT('Ctrl Pts',(-6.13344795559226,-2.94807981291136,
7.16947389713427));
#15440=CARTESIAN_POINT('Ctrl Pts',(-6.67832238690478,-3.17303200251925,
7.24794018550211));
#15441=CARTESIAN_POINT('Ctrl Pts',(-7.02275755554972,-3.65745608532185,
7.32707217829837));
#15442=CARTESIAN_POINT('Ctrl Pts',(-7.05735272280787,-4.25586588177759,
7.40686459608773));
#15443=CARTESIAN_POINT('Ctrl Pts',(-6.76547691196073,-4.78509631171363,
7.48730845620322));
#15444=CARTESIAN_POINT('Ctrl Pts',(-6.2328288010233,-5.08025350877579,7.56837885030285));
#15445=CARTESIAN_POINT('Ctrl Pts',(-5.62013899574997,-5.04649817639357,
7.65005990391116));
#15446=CARTESIAN_POINT('Ctrl Pts',(-5.11580807772359,-4.68938066411544,
7.73232656442466));
#15447=CARTESIAN_POINT('Ctrl Pts',(-4.87715382894508,-4.11483016176644,
7.81515220419497));
#15448=CARTESIAN_POINT('Ctrl Pts',(-4.98155491462679,-3.49739611646809,
7.89850731279159));
#15449=CARTESIAN_POINT('Ctrl Pts',(-5.40077901066439,-3.02758330352059,
7.9823562570568));
#15450=CARTESIAN_POINT('Ctrl Pts',(-6.00943808507216,-2.85154636954707,
8.06666859923912));
#15451=CARTESIAN_POINT('Ctrl Pts',(-6.51885903425478,-2.99816547885978,
8.1372658921751));
#15452=CARTESIAN_POINT('Ctrl Pts',(-6.83430571931979,-3.26544902128311,
8.19393687266448));
#15453=CARTESIAN_POINT('Ctrl Pts',(-7.05200749163975,-3.59028903861244,
8.24756779276489));
#15454=CARTESIAN_POINT('Ctrl Pts',(-7.14819755856945,-4.06384168275982,
8.31243236873047));
#15455=CARTESIAN_POINT('Ctrl Pts',(-6.98081900179575,-4.60598695891977,
8.38858547422415));
#15456=CARTESIAN_POINT('Ctrl Pts',(-6.60788861986765,-4.97019026806658,
8.458578331888));
#15457=CARTESIAN_POINT('Ctrl Pts',(-6.16543359160979,-5.12466006881932,
8.52232968915992));
#15458=CARTESIAN_POINT('Ctrl Pts',(-5.74359928719466,-5.10906351708155,
8.57978479808564));
#15459=CARTESIAN_POINT('Ctrl Pts',(-5.35619714417686,-4.93996484898772,
8.63729543753528));
#15460=CARTESIAN_POINT('Ctrl Pts',(-5.05707781940967,-4.64089287126633,
8.69485958085149));
#15461=CARTESIAN_POINT('Ctrl Pts',(-4.8877873605468,-4.25294305694932,8.7524561265159));
#15462=CARTESIAN_POINT('Ctrl Pts',(-4.87196688005146,-3.8298677000771,8.81006949812648));
#15463=CARTESIAN_POINT('Ctrl Pts',(-5.01177613480597,-3.43021110565367,
8.86768635580782));
#15464=CARTESIAN_POINT('Ctrl Pts',(-5.28787582930203,-3.10936002434098,
8.92528196146821));
#15465=CARTESIAN_POINT('Ctrl Pts',(-5.6619879756221,-2.91181444586473,8.98285200706347));
#15466=CARTESIAN_POINT('Ctrl Pts',(-6.08207592029199,-2.86437706798175,
9.04037821761112));
#15467=CARTESIAN_POINT('Ctrl Pts',(-6.4899603572735,-2.97385511423952,9.09784598588914));
#15468=CARTESIAN_POINT('Ctrl Pts',(-6.82936497495859,-3.22425165825059,
9.15523814001513));
#15469=CARTESIAN_POINT('Ctrl Pts',(-7.053352906295,-3.58086467861269,9.21254084633562));
#15470=CARTESIAN_POINT('Ctrl Pts',(-7.1313961994424,-3.99398472975135,9.26974226638222));
#15471=CARTESIAN_POINT('Ctrl Pts',(-7.0532945194083,-4.40605187892761,9.32682226439619));
#15472=CARTESIAN_POINT('Ctrl Pts',(-6.80592167656756,-4.800012570465,9.39010214047278));
#15473=CARTESIAN_POINT('Ctrl Pts',(-6.37170927836265,-5.08039142951602,
9.4594993944269));
#15474=CARTESIAN_POINT('Ctrl Pts',(-5.81130091232871,-5.12219506735395,
9.53491939194941));
#15475=CARTESIAN_POINT('Ctrl Pts',(-5.28006160362083,-4.88227948380037,
9.61315239896851));
#15476=CARTESIAN_POINT('Ctrl Pts',(-4.92834155153614,-4.38622356770561,
9.69411365299844));
#15477=CARTESIAN_POINT('Ctrl Pts',(-4.89371133000185,-3.75906326920876,
9.77771093250303));
#15478=CARTESIAN_POINT('Ctrl Pts',(-5.19608243373045,-3.21309740789018,
9.86079489873814));
#15479=CARTESIAN_POINT('Ctrl Pts',(-5.73908153611128,-2.91364502826735,
9.94333398508595));
#15480=CARTESIAN_POINT('Ctrl Pts',(-6.35384329508302,-2.94879350552204,
10.0252993757984));
#15481=CARTESIAN_POINT('Ctrl Pts',(-6.85201080049535,-3.30303898937477,
10.1066658330264));
#15482=CARTESIAN_POINT('Ctrl Pts',(-7.08354371570412,-3.8637384379288,10.187411539775));
#15483=CARTESIAN_POINT('Ctrl Pts',(-6.98206687823625,-4.45694888176359,
10.2675183757904));
#15484=CARTESIAN_POINT('Ctrl Pts',(-6.58379226485485,-4.90158283744291,
10.3469719800326));
#15485=CARTESIAN_POINT('Ctrl Pts',(-6.01478871597461,-5.06478222276206,
10.425761837779));
#15486=CARTESIAN_POINT('Ctrl Pts',(-5.4510073752914,-4.90162602393077,10.5038813791205));
#15487=CARTESIAN_POINT('Ctrl Pts',(-5.06381325555816,-4.46729226158387,
10.581327909048));
#15488=CARTESIAN_POINT('Ctrl Pts',(-4.96788652492998,-3.89849834310758,
10.6581028737864));
#15489=CARTESIAN_POINT('Ctrl Pts',(-5.18737077761513,-3.37046753371988,
10.7342112682679));
#15490=CARTESIAN_POINT('Ctrl Pts',(-5.65010527122599,-3.04297938717396,
10.809662885546));
#15491=CARTESIAN_POINT('Ctrl Pts',(-6.21136781157978,-3.01214055539693,
10.88446936741));
#15492=CARTESIAN_POINT('Ctrl Pts',(-6.69883486154469,-3.28231382194347,
10.9586505197816));
#15493=CARTESIAN_POINT('Ctrl Pts',(-6.96586193433289,-3.7664841398465,11.032219855093));
#15494=CARTESIAN_POINT('Ctrl Pts',(-6.93424119916699,-4.31399510918003,
11.1052163057123));
#15495=CARTESIAN_POINT('Ctrl Pts',(-6.61896949124829,-4.75764538304451,
11.1776579397094));
#15496=CARTESIAN_POINT('Ctrl Pts',(-6.11951941708001,-4.96387158643751,
11.2495798113469));
#15497=CARTESIAN_POINT('Ctrl Pts',(-5.59058419165622,-4.87376112739787,
11.3209980698462));
#15498=CARTESIAN_POINT('Ctrl Pts',(-5.19326858782592,-4.51762113802504,
11.3919960114712));
#15499=CARTESIAN_POINT('Ctrl Pts',(-5.09580224443524,-4.17887730357393,
11.4389949666357));
#15500=CARTESIAN_POINT('Ctrl Pts',(-5.0957793236035,-4.00861533013479,11.462499928691));
#15501=CARTESIAN_POINT('Ctrl Pts',(-4.91064566239329,-3.99023206485658,
2.62933152433034));
#15502=CARTESIAN_POINT('Ctrl Pts',(-4.91067312952917,-3.78619909336401,
2.6574986314607));
#15503=CARTESIAN_POINT('Ctrl Pts',(-5.02774343284091,-3.37929348062033,
2.71396207002513));
#15504=CARTESIAN_POINT('Ctrl Pts',(-5.50406153736764,-2.95270955038751,
2.79904101242933));
#15505=CARTESIAN_POINT('Ctrl Pts',(-6.13658014707958,-2.84513696154089,
2.88444997261576));
#15506=CARTESIAN_POINT('Ctrl Pts',(-6.73146552788189,-3.09119886279762,
2.97014767722273));
#15507=CARTESIAN_POINT('Ctrl Pts',(-7.10528990058372,-3.61770798806037,
3.05608468313627));
#15508=CARTESIAN_POINT('Ctrl Pts',(-7.14159326599711,-4.26367257300153,
3.14221376787915));
#15509=CARTESIAN_POINT('Ctrl Pts',(-6.82847203577308,-4.83116825369024,
3.22848316885409));
#15510=CARTESIAN_POINT('Ctrl Pts',(-6.26047894253337,-5.14498395627411,
3.31484078206362));
#15511=CARTESIAN_POINT('Ctrl Pts',(-5.61243809982754,-5.10862883176423,
3.40123876915193));
#15512=CARTESIAN_POINT('Ctrl Pts',(-5.08312065999899,-4.73301532006664,
3.48762383998782));
#15513=CARTESIAN_POINT('Ctrl Pts',(-4.83503964180896,-4.13383055473192,
3.57394517138351));
#15514=CARTESIAN_POINT('Ctrl Pts',(-4.94365798236383,-3.4953620072643,3.66015124298089));
#15515=CARTESIAN_POINT('Ctrl Pts',(-5.37453812537608,-3.01351481306622,
3.7461917900401));
#15516=CARTESIAN_POINT('Ctrl Pts',(-5.99415503872227,-2.8352869923604,3.83201719977587));
#15517=CARTESIAN_POINT('Ctrl Pts',(-6.61176789561045,-3.01349565884922,
3.91757953433049));
#15518=CARTESIAN_POINT('Ctrl Pts',(-7.02236019753619,-3.47368176991699,
3.99967428100357));
#15519=CARTESIAN_POINT('Ctrl Pts',(-7.11918698593408,-3.95609727910189,
4.06572145278173));
#15520=CARTESIAN_POINT('Ctrl Pts',(-7.06340476330875,-4.27068165104005,
4.10961546484208));
#15521=CARTESIAN_POINT('Ctrl Pts',(-6.99930031338402,-4.44014487854788,
4.13465662034055));
#15522=CARTESIAN_POINT('Ctrl Pts',(-6.87255985096034,-4.68025839089964,
4.17217691756027));
#15523=CARTESIAN_POINT('Ctrl Pts',(-6.57315958771661,-4.97217030656539,
4.22830532196756));
#15524=CARTESIAN_POINT('Ctrl Pts',(-6.03903268776397,-5.12206247506981,
4.30276796426334));
#15525=CARTESIAN_POINT('Ctrl Pts',(-5.50097125621371,-4.99896308035578,
4.37684131892625));
#15526=CARTESIAN_POINT('Ctrl Pts',(-5.12440241748786,-4.66549566032703,
4.44436512761515));
#15527=CARTESIAN_POINT('Ctrl Pts',(-4.94538675915755,-4.2540197256944,4.50542676119247));
#15528=CARTESIAN_POINT('Ctrl Pts',(-4.930305222757,-3.85224640541355,4.56013153880702));
#15529=CARTESIAN_POINT('Ctrl Pts',(-5.06282577996349,-3.47483689360371,
4.61457310279514));
#15530=CARTESIAN_POINT('Ctrl Pts',(-5.35125009676625,-3.1392746316074,4.67476651041697));
#15531=CARTESIAN_POINT('Ctrl Pts',(-5.79829809966802,-2.93804410501286,
4.74058503688818));
#15532=CARTESIAN_POINT('Ctrl Pts',(-6.32807786867545,-2.97826387006224,
4.81188334316262));
#15533=CARTESIAN_POINT('Ctrl Pts',(-6.67840551830293,-3.20520787794476,
4.86793768919777));
#15534=CARTESIAN_POINT('Ctrl Pts',(-6.8595784600443,-3.44180802446728,4.90902136435057));
#15535=CARTESIAN_POINT('Ctrl Pts',(-6.974492766904,-3.66912329852776,4.94413862211746));
#15536=CARTESIAN_POINT('Ctrl Pts',(-7.0340823464101,-3.98480672906872,4.9878512860272));
#15537=CARTESIAN_POINT('Ctrl Pts',(-6.96250196758772,-4.36134912898132,
5.04001006483621));
#15538=CARTESIAN_POINT('Ctrl Pts',(-6.75962908600506,-4.68404810660973,
5.09187209661467));
#15539=CARTESIAN_POINT('Ctrl Pts',(-6.45462282106343,-4.90873382172561,
5.14343601874352));
#15540=CARTESIAN_POINT('Ctrl Pts',(-6.09052764960782,-5.00629817643789,
5.19470121102102));
#15541=CARTESIAN_POINT('Ctrl Pts',(-5.71867585943879,-4.96385753221553,
5.24566987862147));
#15542=CARTESIAN_POINT('Ctrl Pts',(-5.27869458048482,-4.73250913068639,
5.31323392862732));
#15543=CARTESIAN_POINT('Ctrl Pts',(-4.95510149885895,-4.17152363114175,
5.39697303342324));
#15544=CARTESIAN_POINT('Ctrl Pts',(-5.12826577922076,-3.42039982727572,
5.49631984882234));
#15545=CARTESIAN_POINT('Ctrl Pts',(-5.65279054674189,-3.06549368105792,
5.5782074053157));
#15546=CARTESIAN_POINT('Ctrl Pts',(-6.1304657902261,-3.04944345002014,5.64319497079561));
#15547=CARTESIAN_POINT('Ctrl Pts',(-6.50414037104288,-3.17959458133367,
5.69707394622442));
#15548=CARTESIAN_POINT('Ctrl Pts',(-6.81832653237479,-3.4864294509472,5.75599775305137));
#15549=CARTESIAN_POINT('Ctrl Pts',(-6.95798781236734,-3.94133529255923,
5.81987492310173));
#15550=CARTESIAN_POINT('Ctrl Pts',(-6.86406020442495,-4.40486030892628,
5.88336458908467));
#15551=CARTESIAN_POINT('Ctrl Pts',(-6.56145066300743,-4.76499099454252,
5.94650053783697));
#15552=CARTESIAN_POINT('Ctrl Pts',(-6.12579690342053,-4.93562462938296,
6.00930535589766));
#15553=CARTESIAN_POINT('Ctrl Pts',(-5.70231406382442,-4.88235175336122,
6.06660462669795));
#15554=CARTESIAN_POINT('Ctrl Pts',(-5.37955587569654,-4.67904760710474,
6.11850018003562));
#15555=CARTESIAN_POINT('Ctrl Pts',(-5.17633016181025,-4.40380143225806,
6.16506396148214));
#15556=CARTESIAN_POINT('Ctrl Pts',(-5.08810842094241,-4.07402072845824,
6.21150782441348));
#15557=CARTESIAN_POINT('Ctrl Pts',(-5.12629567820714,-3.73567498665909,
6.25783953958017));
#15558=CARTESIAN_POINT('Ctrl Pts',(-5.28511244198756,-3.43529706348013,
6.30407622395686));
#15559=CARTESIAN_POINT('Ctrl Pts',(-5.54229551854319,-3.21398520007125,
6.35023138483534));
#15560=CARTESIAN_POINT('Ctrl Pts',(-5.8619107236865,-3.10233975226692,6.39632010313442));
#15561=CARTESIAN_POINT('Ctrl Pts',(-6.25663673452835,-3.11661537197105,
6.45003081505834));
#15562=CARTESIAN_POINT('Ctrl Pts',(-6.65960184073881,-3.33909366935506,
6.51135170134586));
#15563=CARTESIAN_POINT('Ctrl Pts',(-6.9103998303242,-3.79306634470867,6.58031178132487));
#15564=CARTESIAN_POINT('Ctrl Pts',(-6.88609075922184,-4.22370084373278,
6.63779351550458));
#15565=CARTESIAN_POINT('Ctrl Pts',(-6.73144911525362,-4.5221338311146,6.6838161310143));
#15566=CARTESIAN_POINT('Ctrl Pts',(-6.5394091300997,-4.72493928671578,6.72219558958497));
#15567=CARTESIAN_POINT('Ctrl Pts',(-6.16486636586928,-4.92501555623377,
6.77982471041186));
#15568=CARTESIAN_POINT('Ctrl Pts',(-5.63103734380132,-4.88518117432037,
6.84913849179702));
#15569=CARTESIAN_POINT('Ctrl Pts',(-5.19737626012191,-4.49646149289223,
6.92644120860721));
#15570=CARTESIAN_POINT('Ctrl Pts',(-5.0518312613499,-3.99310443836122,6.99628668811257));
#15571=CARTESIAN_POINT('Ctrl Pts',(-5.1977151858362,-3.48623546915741,7.06644859462949));
#15572=CARTESIAN_POINT('Ctrl Pts',(-5.59236675555469,-3.13299752231314,
7.13697518250154));
#15573=CARTESIAN_POINT('Ctrl Pts',(-6.11768012047296,-3.04324969507249,
7.2079058054426));
#15574=CARTESIAN_POINT('Ctrl Pts',(-6.61330050675189,-3.24802636853269,
7.27928132209));
#15575=CARTESIAN_POINT('Ctrl Pts',(-6.92601453710887,-3.68801965644784,
7.35114007330658));
#15576=CARTESIAN_POINT('Ctrl Pts',(-6.95734111922486,-4.23086268142858,
7.42351372630332));
#15577=CARTESIAN_POINT('Ctrl Pts',(-6.69270416831019,-4.71067464476414,
7.49643069526812));
#15578=CARTESIAN_POINT('Ctrl Pts',(-6.20975100340118,-4.97833378740792,
7.56992638519204));
#15579=CARTESIAN_POINT('Ctrl Pts',(-5.65383497595805,-4.94778246347922,
7.64402199805137));
#15580=CARTESIAN_POINT('Ctrl Pts',(-5.19560892172118,-4.62346526629037,
7.71873991750681));
#15581=CARTESIAN_POINT('Ctrl Pts',(-4.97826933155121,-4.10067068964125,
7.79409718811368));
#15582=CARTESIAN_POINT('Ctrl Pts',(-5.0732790960684,-3.53747137568016,7.87010685457802));
#15583=CARTESIAN_POINT('Ctrl Pts',(-5.45652751621272,-3.10760420604816,
7.94678031881255));
#15584=CARTESIAN_POINT('Ctrl Pts',(-6.01492249584954,-2.94579389365945,
8.02411893674303));
#15585=CARTESIAN_POINT('Ctrl Pts',(-6.48419486025271,-3.08058022325691,
8.08913615817866));
#15586=CARTESIAN_POINT('Ctrl Pts',(-6.77567109544999,-3.32746414120783,
8.14148107252939));
#15587=CARTESIAN_POINT('Ctrl Pts',(-6.97726832362751,-3.62817763584748,
8.19113027512342));
#15588=CARTESIAN_POINT('Ctrl Pts',(-7.06683150986179,-4.06785942369035,
8.25133905297887));
#15589=CARTESIAN_POINT('Ctrl Pts',(-6.91099271737997,-4.57359787784397,
8.32235695721035));
#15590=CARTESIAN_POINT('Ctrl Pts',(-6.56180322265575,-4.91501872365941,
8.38791913097088));
#15591=CARTESIAN_POINT('Ctrl Pts',(-6.1455889673863,-5.06048615843406,8.44788148951164));
#15592=CARTESIAN_POINT('Ctrl Pts',(-5.74726405458259,-5.045901194332,8.5021199776848));
#15593=CARTESIAN_POINT('Ctrl Pts',(-5.37997014596406,-4.88573433422684,
8.55663032383165));
#15594=CARTESIAN_POINT('Ctrl Pts',(-5.09521606139379,-4.60124328031376,
8.61139619541384));
#15595=CARTESIAN_POINT('Ctrl Pts',(-4.93332552837962,-4.23064059662876,
8.66641388088589));
#15596=CARTESIAN_POINT('Ctrl Pts',(-4.9179903715202,-3.82475321029841,8.72167508913329));
#15597=CARTESIAN_POINT('Ctrl Pts',(-5.05253490297233,-3.43967511432446,
8.777169282374));
#15598=CARTESIAN_POINT('Ctrl Pts',(-5.31955851270096,-3.12911022044219,
8.8328932111667));
#15599=CARTESIAN_POINT('Ctrl Pts',(-5.68303528443618,-2.93700186151765,
8.88882890536203));
#15600=CARTESIAN_POINT('Ctrl Pts',(-6.09302465655479,-2.89052402217789,
8.94496765237401));
#15601=CARTESIAN_POINT('Ctrl Pts',(-6.49294269468231,-2.99769732695354,
9.00129753538956));
#15602=CARTESIAN_POINT('Ctrl Pts',(-6.82727292776362,-3.24413114332201,
9.05780821017147));
#15603=CARTESIAN_POINT('Ctrl Pts',(-7.04898730088169,-3.59680786031477,
9.11448652506239));
#15604=CARTESIAN_POINT('Ctrl Pts',(-7.12670330693309,-4.00728190088154,
9.17131792719747));
#15605=CARTESIAN_POINT('Ctrl Pts',(-7.04890710360552,-4.41865064133336,
9.22829293049541));
#15606=CARTESIAN_POINT('Ctrl Pts',(-6.80102480792446,-4.81378239727149,
9.29173772436838));
#15607=CARTESIAN_POINT('Ctrl Pts',(-6.36351538644652,-5.09674069553992,
9.36169115447804));
#15608=CARTESIAN_POINT('Ctrl Pts',(-5.7952165870531,-5.1395532745806,9.43816998078719));
#15609=CARTESIAN_POINT('Ctrl Pts',(-5.25307378945426,-4.89518090505499,
9.51797249895571));
#15610=CARTESIAN_POINT('Ctrl Pts',(-4.89153837004136,-4.38624542537144,
9.60108046017307));
#15611=CARTESIAN_POINT('Ctrl Pts',(-4.85517495180513,-3.73819432300457,
9.68745784720193));
#15612=CARTESIAN_POINT('Ctrl Pts',(-5.16914448740319,-3.17012933555682,
9.77385698474107));
#15613=CARTESIAN_POINT('Ctrl Pts',(-5.73710541159327,-2.85628563202139,
9.86022602760031));
#15614=CARTESIAN_POINT('Ctrl Pts',(-6.38433613751579,-2.89276199039655,
9.94651355241989));
#15615=CARTESIAN_POINT('Ctrl Pts',(-6.91212050930184,-3.26744932078839,
10.0326685712732));
#15616=CARTESIAN_POINT('Ctrl Pts',(-7.15908057305555,-3.86425638646486,
10.1186409109809));
#15617=CARTESIAN_POINT('Ctrl Pts',(-7.05091161244937,-4.49924587495838,
10.2043814658325));
#15618=CARTESIAN_POINT('Ctrl Pts',(-6.62285185241079,-4.97775602995875,
10.2898425301769));
#15619=CARTESIAN_POINT('Ctrl Pts',(-6.00816341099947,-5.15445618405033,
10.3749780585446));
#15620=CARTESIAN_POINT('Ctrl Pts',(-5.39636763024784,-4.97776483774591,
10.4597439223075));
#15621=CARTESIAN_POINT('Ctrl Pts',(-4.97444985106601,-4.50494216067592,
10.5440982117258));
#15622=CARTESIAN_POINT('Ctrl Pts',(-4.86936608454769,-3.88345546663721,
10.62800140343));
#15623=CARTESIAN_POINT('Ctrl Pts',(-5.10968162167462,-3.30472800962943,
10.7114168360999));
#15624=CARTESIAN_POINT('Ctrl Pts',(-5.61787204048362,-2.94485337288711,
10.7943103120336));
#15625=CARTESIAN_POINT('Ctrl Pts',(-6.23553216372117,-2.91079260460954,
10.8766517425954));
#15626=CARTESIAN_POINT('Ctrl Pts',(-6.77273785370402,-3.20844608120544,
10.9584121473814));
#15627=CARTESIAN_POINT('Ctrl Pts',(-7.06723015563896,-3.74240199207279,
11.0395709595654));
#15628=CARTESIAN_POINT('Ctrl Pts',(-7.03232554389622,-4.34631413758613,
11.1201002984029));
#15629=CARTESIAN_POINT('Ctrl Pts',(-6.6846440480935,-4.83541725513737,11.1999834703407));
#15630=CARTESIAN_POINT('Ctrl Pts',(-6.13443860678649,-5.06246468337482,
11.2792177855247));
#15631=CARTESIAN_POINT('Ctrl Pts',(-5.55273853859017,-4.96317392286291,
11.3577768015645));
#15632=CARTESIAN_POINT('Ctrl Pts',(-5.11687440986545,-4.57225551739733,
11.4356905379074));
#15633=CARTESIAN_POINT('Ctrl Pts',(-5.01030571579522,-4.20147270550581,
11.4871432816273));
#15634=CARTESIAN_POINT('Ctrl Pts',(-5.0102806896419,-4.01557184907574,11.5128072187248));
#15635=CARTESIAN_POINT('Ctrl Pts',(-4.97008191124373,-3.98632049867421,
2.60093950625047));
#15636=CARTESIAN_POINT('Ctrl Pts',(-4.97010792325046,-3.79309660191043,
2.62761440178562));
#15637=CARTESIAN_POINT('Ctrl Pts',(-5.08090684239098,-3.40768944058894,
2.68109048286901));
#15638=CARTESIAN_POINT('Ctrl Pts',(-5.53323464929853,-3.00219742821615,
2.76192326014508));
#15639=CARTESIAN_POINT('Ctrl Pts',(-6.13583253713359,-2.89947156896757,
2.84329266550979));
#15640=CARTESIAN_POINT('Ctrl Pts',(-6.70452266565683,-3.13436261802716,
2.92520197170544));
#15641=CARTESIAN_POINT('Ctrl Pts',(-7.06328708852698,-3.63910731072172,
3.00761448887057));
#15642=CARTESIAN_POINT('Ctrl Pts',(-7.09856063711344,-4.26079276792185,
3.09050857590128));
#15643=CARTESIAN_POINT('Ctrl Pts',(-6.79637837460094,-4.80919935005163,
3.17384771454092));
#15644=CARTESIAN_POINT('Ctrl Pts',(-6.24569012974855,-5.11388530829306,
3.25759626910264));
#15645=CARTESIAN_POINT('Ctrl Pts',(-5.61459646028545,-5.07886298559536,
3.34172561849207));
#15646=CARTESIAN_POINT('Ctrl Pts',(-5.09674658023812,-4.71186793716836,
3.4261938545368));
#15647=CARTESIAN_POINT('Ctrl Pts',(-4.85272822511499,-4.1235468329122,3.51096209906644));
#15648=CARTESIAN_POINT('Ctrl Pts',(-4.95946885344308,-3.49366428571328,
3.59598755345742));
#15649=CARTESIAN_POINT('Ctrl Pts',(-5.3860925399307,-3.01594593450921,3.6812267005334));
#15650=CARTESIAN_POINT('Ctrl Pts',(-6.00269019835541,-2.83814374866598,
3.76663475578024));
#15651=CARTESIAN_POINT('Ctrl Pts',(-6.62031834420698,-3.01590617483508,
3.8521649675602));
#15652=CARTESIAN_POINT('Ctrl Pts',(-7.03301623099344,-3.4778365045598,3.93460141464829));
#15653=CARTESIAN_POINT('Ctrl Pts',(-7.13093805843655,-3.96439424471186,
4.00120453997466));
#15654=CARTESIAN_POINT('Ctrl Pts',(-7.07454128905103,-4.28269736823964,
4.04560964054819));
#15655=CARTESIAN_POINT('Ctrl Pts',(-7.00958861255911,-4.45442131099228,
4.07098282756962));
#15656=CARTESIAN_POINT('Ctrl Pts',(-6.88104498689409,-4.69797936078498,
4.10903813285862));
#15657=CARTESIAN_POINT('Ctrl Pts',(-6.57682855326753,-4.99492524656468,
4.1660763537331));
#15658=CARTESIAN_POINT('Ctrl Pts',(-6.0316469704085,-5.14822432672608,4.24208367835567));
#15659=CARTESIAN_POINT('Ctrl Pts',(-5.48021578029777,-5.02235110130459,
4.3179748190391));
#15660=CARTESIAN_POINT('Ctrl Pts',(-5.09271529118042,-4.6795516092149,4.38740377644772));
#15661=CARTESIAN_POINT('Ctrl Pts',(-4.90786994693549,-4.25495657649653,
4.45041036428995));
#15662=CARTESIAN_POINT('Ctrl Pts',(-4.89214664286788,-3.83924497527109,
4.50699930620379));
#15663=CARTESIAN_POINT('Ctrl Pts',(-5.02955352183774,-3.44765692035231,
4.56346991950519));
#15664=CARTESIAN_POINT('Ctrl Pts',(-5.32945197831939,-3.09855693967571,
4.62606391022856));
#15665=CARTESIAN_POINT('Ctrl Pts',(-5.79573806357998,-2.88844341511611,
4.69471397223731));
#15666=CARTESIAN_POINT('Ctrl Pts',(-6.35019247867269,-2.93031759176993,
4.76932252526924));
#15667=CARTESIAN_POINT('Ctrl Pts',(-6.71791383824202,-3.16834791049732,
4.82810753382221));
#15668=CARTESIAN_POINT('Ctrl Pts',(-6.90847162726572,-3.41718092381109,
4.87131014132301));
#15669=CARTESIAN_POINT('Ctrl Pts',(-7.02945840397545,-3.65648859532012,
4.90827460291562));
#15670=CARTESIAN_POINT('Ctrl Pts',(-7.09235415647436,-3.98932316476188,
4.95435468147015));
#15671=CARTESIAN_POINT('Ctrl Pts',(-7.01679613358752,-4.38709288630926,
5.00944049543375));
#15672=CARTESIAN_POINT('Ctrl Pts',(-6.80218102266994,-4.72860976063846,
5.06430748189597));
#15673=CARTESIAN_POINT('Ctrl Pts',(-6.47891565083903,-4.96679436777757,
5.11894822582177));
#15674=CARTESIAN_POINT('Ctrl Pts',(-6.09242502205773,-5.07042049311667,
5.17335860716689));
#15675=CARTESIAN_POINT('Ctrl Pts',(-5.69712814211187,-5.02533685252607,
5.22752916796423));
#15676=CARTESIAN_POINT('Ctrl Pts',(-5.22881038622497,-4.77916247689946,
5.29943193022554));
#15677=CARTESIAN_POINT('Ctrl Pts',(-4.8836815835944,-4.18127755734618,5.38866309511102));
#15678=CARTESIAN_POINT('Ctrl Pts',(-5.06839094832227,-3.37929873201119,
5.49470580468442));
#15679=CARTESIAN_POINT('Ctrl Pts',(-5.62883774530645,-3.00003776994351,
5.58217611826977));
#15680=CARTESIAN_POINT('Ctrl Pts',(-6.13932551294608,-2.98290693407233,
5.65161646350273));
#15681=CARTESIAN_POINT('Ctrl Pts',(-6.53861788941739,-3.12198633810778,
5.70918134513565));
#15682=CARTESIAN_POINT('Ctrl Pts',(-6.8742032976184,-3.4497749510831,5.77211341790662));
#15683=CARTESIAN_POINT('Ctrl Pts',(-7.02320804724903,-3.93535711597183,
5.84028217731445));
#15684=CARTESIAN_POINT('Ctrl Pts',(-6.92297139477486,-4.42960801271712,
5.90797662474841));
#15685=CARTESIAN_POINT('Ctrl Pts',(-6.60065686050615,-4.81301742724568,
5.97519783526073));
#15686=CARTESIAN_POINT('Ctrl Pts',(-6.13749803630879,-4.99428816457585,
6.04195679074869));
#15687=CARTESIAN_POINT('Ctrl Pts',(-5.68826175552714,-4.9376390353816,6.1027374472312));
#15688=CARTESIAN_POINT('Ctrl Pts',(-5.34662282232589,-4.7223338410458,6.15767181180174));
#15689=CARTESIAN_POINT('Ctrl Pts',(-5.13194361739086,-4.43145703525003,
6.20687182350689));
#15690=CARTESIAN_POINT('Ctrl Pts',(-5.03901270494996,-4.08371896980411,
6.25583828963203));
#15691=CARTESIAN_POINT('Ctrl Pts',(-5.07927303344496,-3.72779634187791,
6.30457776363547));
#15692=CARTESIAN_POINT('Ctrl Pts',(-5.24602249926503,-3.41261874140077,
6.35309845686694));
#15693=CARTESIAN_POINT('Ctrl Pts',(-5.5152804095074,-3.1810516668998,6.40140936712654));
#15694=CARTESIAN_POINT('Ctrl Pts',(-5.84893154516085,-3.06460741415626,
6.44951841989009));
#15695=CARTESIAN_POINT('Ctrl Pts',(-6.25977592394247,-3.07960237391109,
6.50542489105098));
#15696=CARTESIAN_POINT('Ctrl Pts',(-6.67746012847371,-3.31055664624366,
6.56900781660853));
#15697=CARTESIAN_POINT('Ctrl Pts',(-6.93590942148792,-3.77925425753501,
6.64018638784732));
#15698=CARTESIAN_POINT('Ctrl Pts',(-6.91063838592921,-4.22138495835218,
6.69920846194775));
#15699=CARTESIAN_POINT('Ctrl Pts',(-6.75240356125144,-4.52656025392589,
6.74628493506968));
#15700=CARTESIAN_POINT('Ctrl Pts',(-6.55648751063966,-4.73340807548516,
6.78543807765367));
#15701=CARTESIAN_POINT('Ctrl Pts',(-6.17549659731643,-4.93670212163746,
6.84404533283986));
#15702=CARTESIAN_POINT('Ctrl Pts',(-5.63568864954653,-4.89574010065246,
6.91414579643729));
#15703=CARTESIAN_POINT('Ctrl Pts',(-5.20029791031333,-4.50472944721903,
6.99184586086499));
#15704=CARTESIAN_POINT('Ctrl Pts',(-5.05524611097297,-4.0016492232368,7.06165065576445));
#15705=CARTESIAN_POINT('Ctrl Pts',(-5.20062622496947,-3.49805247371584,
7.13139550084469));
#15706=CARTESIAN_POINT('Ctrl Pts',(-5.59091658743601,-3.14926506675406,
7.20110582590366));
#15707=CARTESIAN_POINT('Ctrl Pts',(-6.10736329715364,-3.06142476350215,
7.27084568737173));
#15708=CARTESIAN_POINT('Ctrl Pts',(-6.59186085954437,-3.26202265988594,
7.34065571252636));
#15709=CARTESIAN_POINT('Ctrl Pts',(-6.89581340654691,-3.69030143654108,
7.41058101647453));
#15710=CARTESIAN_POINT('Ctrl Pts',(-6.92579082783416,-4.21593899400802,
7.48067473906963));
#15711=CARTESIAN_POINT('Ctrl Pts',(-6.67042532145853,-4.67827675202706,
7.55099101068251));
#15712=CARTESIAN_POINT('Ctrl Pts',(-6.20676421941765,-4.93489381099811,
7.621551806708));
#15713=CARTESIAN_POINT('Ctrl Pts',(-5.67535748365785,-4.90541034209074,
7.69240985629438));
#15714=CARTESIAN_POINT('Ctrl Pts',(-5.23906347903042,-4.5962956089863,7.76360171950934));
#15715=CARTESIAN_POINT('Ctrl Pts',(-5.03295148115901,-4.0998893028727,7.8351675530826));
#15716=CARTESIAN_POINT('Ctrl Pts',(-5.12310040907612,-3.56680199598165,
7.90714445094969));
#15717=CARTESIAN_POINT('Ctrl Pts',(-5.48510203815549,-3.16103430736412,
7.97956372049517));
#15718=CARTESIAN_POINT('Ctrl Pts',(-6.01128256578978,-3.00871765656471,
8.0524644644889));
#15719=CARTESIAN_POINT('Ctrl Pts',(-6.45259276873704,-3.13557676936373,
8.11361809715538));
#15720=CARTESIAN_POINT('Ctrl Pts',(-6.72644062352849,-3.3675500016554,8.16281094434981));
#15721=CARTESIAN_POINT('Ctrl Pts',(-6.91573050923383,-3.64992945061337,
8.20943672508966));
#15722=CARTESIAN_POINT('Ctrl Pts',(-6.9997439667954,-4.06259387267818,8.26596983287103));
#15723=CARTESIAN_POINT('Ctrl Pts',(-6.85357445098635,-4.5369172654714,8.33258593322727));
#15724=CARTESIAN_POINT('Ctrl Pts',(-6.52613326631928,-4.85706075770687,
8.39407600868389));
#15725=CARTESIAN_POINT('Ctrl Pts',(-6.13582429272564,-4.99349511886135,
8.4503205266024));
#15726=CARTESIAN_POINT('Ctrl Pts',(-5.76219860171794,-4.97982687279222,
8.50120815835136));
#15727=CARTESIAN_POINT('Ctrl Pts',(-5.41756394793594,-4.82956789187536,
8.55235995770513));
#15728=CARTESIAN_POINT('Ctrl Pts',(-5.15020706355995,-4.56249213532047,
8.60378685083323));
#15729=CARTESIAN_POINT('Ctrl Pts',(-4.9980806986773,-4.21432615798783,8.65548587532449));
#15730=CARTESIAN_POINT('Ctrl Pts',(-4.98362078138167,-3.83267457667929,
8.70745682142475));
#15731=CARTESIAN_POINT('Ctrl Pts',(-5.11021173610357,-3.47020564084564,
8.75970064885389));
#15732=CARTESIAN_POINT('Ctrl Pts',(-5.36178391702095,-3.17754370452478,
8.81221057010265));
#15733=CARTESIAN_POINT('Ctrl Pts',(-5.70469395829501,-2.99623679778711,
8.86499141460679));
#15734=CARTESIAN_POINT('Ctrl Pts',(-6.09205813677498,-2.95226910744711,
8.91803745092096));
#15735=CARTESIAN_POINT('Ctrl Pts',(-6.47051636999889,-3.05361664512734,
8.9713474017782));
#15736=CARTESIAN_POINT('Ctrl Pts',(-6.78745601078875,-3.2871476120119,9.02491490657847));
#15737=CARTESIAN_POINT('Ctrl Pts',(-6.99804991983352,-3.6219905623486,9.07873698274717));
#15738=CARTESIAN_POINT('Ctrl Pts',(-7.07207026168852,-4.01248712098153,
9.13280775366998));
#15739=CARTESIAN_POINT('Ctrl Pts',(-6.99798838023044,-4.40464589014135,
9.18712123173382));
#15740=CARTESIAN_POINT('Ctrl Pts',(-6.76128106236067,-4.78216208475497,
9.24773154241494));
#15741=CARTESIAN_POINT('Ctrl Pts',(-6.34236359791613,-5.05332459558266,
9.31472994340359));
#15742=CARTESIAN_POINT('Ctrl Pts',(-5.79640293018885,-5.09468728035619,
9.38820557688175));
#15743=CARTESIAN_POINT('Ctrl Pts',(-5.27374807194744,-4.85938295343188,
9.46512285630086));
#15744=CARTESIAN_POINT('Ctrl Pts',(-4.92374139291998,-4.36727160302241,
9.54551374515351));
#15745=CARTESIAN_POINT('Ctrl Pts',(-4.88804833882704,-3.73790823726897,
9.62939856567637));
#15746=CARTESIAN_POINT('Ctrl Pts',(-5.19389456911797,-3.18374459916885,
9.7136487215973));
#15747=CARTESIAN_POINT('Ctrl Pts',(-5.7499262029823,-2.87603897724937,9.79822511636517));
#15748=CARTESIAN_POINT('Ctrl Pts',(-6.38655698857843,-2.91151088221277,
9.88308689374091));
#15749=CARTESIAN_POINT('Ctrl Pts',(-6.90821328840495,-3.28134043117039,
9.96819148980261));
#15750=CARTESIAN_POINT('Ctrl Pts',(-7.15367511216456,-3.87342998538574,
10.0534949279284));
#15751=CARTESIAN_POINT('Ctrl Pts',(-7.04626285151201,-4.50649326011972,
10.1389520349226));
#15752=CARTESIAN_POINT('Ctrl Pts',(-6.61792394699237,-4.98595040081837,
10.2245167629568));
#15753=CARTESIAN_POINT('Ctrl Pts',(-5.99969540032943,-5.16410689978942,
10.3101423900334));
#15754=CARTESIAN_POINT('Ctrl Pts',(-5.38135114053038,-4.98595903034396,
10.3957818820093));
#15755=CARTESIAN_POINT('Ctrl Pts',(-4.95276973155278,-4.50628650839756,
10.4813879625181));
#15756=CARTESIAN_POINT('Ctrl Pts',(-4.84522951556671,-3.87269630342893,
10.5669138370986));
#15757=CARTESIAN_POINT('Ctrl Pts',(-5.09095827763592,-3.27990007927789,
10.6523125070039));
#15758=CARTESIAN_POINT('Ctrl Pts',(-5.61337048591891,-2.90947965858988,
10.7375390455524));
#15759=CARTESIAN_POINT('Ctrl Pts',(-6.2512116652945,-2.8739197839433,10.8225463831617));
#15760=CARTESIAN_POINT('Ctrl Pts',(-6.80839117558467,-3.18222380258799,
10.9072955143056));
#15761=CARTESIAN_POINT('Ctrl Pts',(-7.11523129697893,-3.73778673767215,
10.9917334063949));
#15762=CARTESIAN_POINT('Ctrl Pts',(-7.07909456599979,-4.36871911225707,
11.0758426906577));
#15763=CARTESIAN_POINT('Ctrl Pts',(-6.71487307508494,-4.88164185779045,
11.1595743427241));
#15764=CARTESIAN_POINT('Ctrl Pts',(-6.13633158216785,-5.12070793186404,
11.2428882077646));
#15765=CARTESIAN_POINT('Ctrl Pts',(-5.52270076886875,-5.01618598996208,
11.325745296715));
#15766=CARTESIAN_POINT('Ctrl Pts',(-5.06153326945952,-4.60290245400468,
11.4081370879796));
#15767=CARTESIAN_POINT('Ctrl Pts',(-4.94849818871498,-4.20962129150326,
11.4626969504328));
#15768=CARTESIAN_POINT('Ctrl Pts',(-4.94847164137574,-4.01242066547175,
11.4899208404097));
#15769=CARTESIAN_POINT('Ctrl Pts',(-5.0000018410068,-3.98632452652701,2.60093950625047));
#15770=CARTESIAN_POINT('Ctrl Pts',(-5.00002711936198,-3.79855038268961,
2.62686205390092));
#15771=CARTESIAN_POINT('Ctrl Pts',(-5.10766548646186,-3.42414266353048,
2.67881373981085));
#15772=CARTESIAN_POINT('Ctrl Pts',(-5.54728618664091,-3.02997941177219,
2.75738438838345));
#15773=CARTESIAN_POINT('Ctrl Pts',(-6.13328094577175,-2.93005881251319,
2.83651316903494));
#15774=CARTESIAN_POINT('Ctrl Pts',(-6.68670283260197,-3.15858336118752,
2.91622304878198));
#15775=CARTESIAN_POINT('Ctrl Pts',(-7.03616187921695,-3.65012597802659,
2.99648821676135));
#15776=CARTESIAN_POINT('Ctrl Pts',(-7.07062949516082,-4.25616589762635,
3.07729930317819));
#15777=CARTESIAN_POINT('Ctrl Pts',(-6.77580863517498,-4.79139923899731,
3.15863489698049));
#15778=CARTESIAN_POINT('Ctrl Pts',(-6.23777999713871,-5.08919902934938,
3.24047455745509));
#15779=CARTESIAN_POINT('Ctrl Pts',(-5.62032344264714,-5.05504677509261,
3.32279321070673));
#15780=CARTESIAN_POINT('Ctrl Pts',(-5.11287137916696,-4.69557478020053,
3.40556356877954));
#15781=CARTESIAN_POINT('Ctrl Pts',(-4.87329914702911,-4.11831903637453,
3.48875540125931));
#15782=CARTESIAN_POINT('Ctrl Pts',(-4.97807346419814,-3.49920456570944,
3.57233609900605));
#15783=CARTESIAN_POINT('Ctrl Pts',(-5.39799493781825,-3.02877333945258,
3.65627071903615));
#15784=CARTESIAN_POINT('Ctrl Pts',(-6.00610273172108,-2.85326324045065,
3.74052224127624));
#15785=CARTESIAN_POINT('Ctrl Pts',(-6.61643757836359,-3.02876545098225,
3.82505176791358));
#15786=CARTESIAN_POINT('Ctrl Pts',(-7.02513160270699,-3.48597574268572,
3.90667922493066));
#15787=CARTESIAN_POINT('Ctrl Pts',(-7.12235641775929,-3.9685483460108,3.97275270898905));
#15788=CARTESIAN_POINT('Ctrl Pts',(-7.06636481269846,-4.28466100128236,
4.01685604551847));
#15789=CARTESIAN_POINT('Ctrl Pts',(-7.00182040328561,-4.45530975229043,
4.04207155819959));
#15790=CARTESIAN_POINT('Ctrl Pts',(-6.87402691871924,-4.69744869614318,
4.07990746733096));
#15791=CARTESIAN_POINT('Ctrl Pts',(-6.57124878899927,-4.99309357202046,
4.1367051149187));
#15792=CARTESIAN_POINT('Ctrl Pts',(-6.02768033690931,-5.14605913758532,
4.2124974864954));
#15793=CARTESIAN_POINT('Ctrl Pts',(-5.47679456345111,-5.0204436702095,4.28832048286543));
#15794=CARTESIAN_POINT('Ctrl Pts',(-5.08889541312948,-4.67743201497751,
4.35782392862843));
#15795=CARTESIAN_POINT('Ctrl Pts',(-4.90355272665998,-4.25185719379132,
4.42098501738742));
#15796=CARTESIAN_POINT('Ctrl Pts',(-4.88772422317122,-3.83457870292561,
4.47779828347438));
#15797=CARTESIAN_POINT('Ctrl Pts',(-5.02577825319216,-3.44096047951616,
4.5345666000236));
#15798=CARTESIAN_POINT('Ctrl Pts',(-5.32758243531257,-3.08955719770179,
4.59757801626674));
#15799=CARTESIAN_POINT('Ctrl Pts',(-5.79757132369034,-2.87764760865861,
4.66678930745632));
#15800=CARTESIAN_POINT('Ctrl Pts',(-6.35748141231083,-2.91980778121556,
4.74213608943437));
#15801=CARTESIAN_POINT('Ctrl Pts',(-6.72958410590507,-3.16055362161142,
4.80163845366161));
#15802=CARTESIAN_POINT('Ctrl Pts',(-6.922583408066,-3.41255717151317,4.8453962925926));
#15803=CARTESIAN_POINT('Ctrl Pts',(-7.04520229026909,-3.65506744231538,
4.88286085267916));
#15804=CARTESIAN_POINT('Ctrl Pts',(-7.10903827020174,-3.9926759490213,4.92960885619655));
#15805=CARTESIAN_POINT('Ctrl Pts',(-7.032354492376,-4.39667067923105,4.98556279568034));
#15806=CARTESIAN_POINT('Ctrl Pts',(-6.81415974257675,-4.74396102273289,
5.04136211338037));
#15807=CARTESIAN_POINT('Ctrl Pts',(-6.48510242262688,-4.98648342248571,
5.09699623581333));
#15808=CARTESIAN_POINT('Ctrl Pts',(-6.09122164110091,-5.09213718968761,
5.15245506498449));
#15809=CARTESIAN_POINT('Ctrl Pts',(-5.6879156360413,-5.04618557814476,5.20772889788153));
#15810=CARTESIAN_POINT('Ctrl Pts',(-5.20960410281967,-4.79482820495352,
5.28116853491036));
#15811=CARTESIAN_POINT('Ctrl Pts',(-4.85635661256684,-4.18339627204868,
5.37246079310469));
#15812=CARTESIAN_POINT('Ctrl Pts',(-5.04534497366866,-3.36152922837358,
5.4811368047244));
#15813=CARTESIAN_POINT('Ctrl Pts',(-5.62045222073828,-2.97210695679973,
5.57092649482181));
#15814=CARTESIAN_POINT('Ctrl Pts',(-6.14491401311764,-2.95446524901901,
5.64227218329944));
#15815=CARTESIAN_POINT('Ctrl Pts',(-6.55538629310792,-3.09741218079302,
5.70145206897501));
#15816=CARTESIAN_POINT('Ctrl Pts',(-6.90061904209687,-3.43455608810828,
5.76619150175189));
#15817=CARTESIAN_POINT('Ctrl Pts',(-7.05403180026006,-3.93434682913999,
5.83636208061574));
#15818=CARTESIAN_POINT('Ctrl Pts',(-6.95084370870626,-4.44331194962687,
5.90607316768221));
#15819=CARTESIAN_POINT('Ctrl Pts',(-6.61884201115902,-4.83828819326241,
5.97532164622816));
#15820=CARTESIAN_POINT('Ctrl Pts',(-6.14163977231472,-5.02507153362565,
6.04410658214742));
#15821=CARTESIAN_POINT('Ctrl Pts',(-5.67874308979945,-4.96670943531882,
6.10673565115305));
#15822=CARTESIAN_POINT('Ctrl Pts',(-5.32673727495899,-4.74487796933182,
6.16333654805419));
#15823=CARTESIAN_POINT('Ctrl Pts',(-5.10557737295403,-4.44521639081723,
6.21402149420468));
#15824=CARTESIAN_POINT('Ctrl Pts',(-5.00986236436416,-4.08706033297606,
6.26445344628883));
#15825=CARTESIAN_POINT('Ctrl Pts',(-5.05132140869747,-3.72058500062059,
6.31463598386295));
#15826=CARTESIAN_POINT('Ctrl Pts',(-5.22295427342147,-3.39619318419661,
6.36457331207659));
#15827=CARTESIAN_POINT('Ctrl Pts',(-5.49996349858563,-3.15797332202467,
6.41427030413784));
#15828=CARTESIAN_POINT('Ctrl Pts',(-5.843023257891,-3.03825996963253,6.46373244033231));
#15829=CARTESIAN_POINT('Ctrl Pts',(-6.2651798733637,-3.05368284090179,6.52117143934356));
#15830=CARTESIAN_POINT('Ctrl Pts',(-6.69395218073661,-3.29085487418832,
6.58644589644131));
#15831=CARTESIAN_POINT('Ctrl Pts',(-6.9588514090406,-3.77142724594311,6.65940509135759));
#15832=CARTESIAN_POINT('Ctrl Pts',(-6.93289301903251,-4.22410112506723,
6.71983222544231));
#15833=CARTESIAN_POINT('Ctrl Pts',(-6.77106481048377,-4.53615877260298,
6.76796591761938));
#15834=CARTESIAN_POINT('Ctrl Pts',(-6.57088599598262,-4.74749645053629,
6.8079662999785));
#15835=CARTESIAN_POINT('Ctrl Pts',(-6.18196007039062,-4.95496402481898,
6.86778079666891));
#15836=CARTESIAN_POINT('Ctrl Pts',(-5.63200940413013,-4.91297894303413,
6.93919834468442));
#15837=CARTESIAN_POINT('Ctrl Pts',(-5.18963313111942,-4.51545599119052,
7.01814869825501));
#15838=CARTESIAN_POINT('Ctrl Pts',(-5.04266994609727,-4.00519996765647,
7.08893288548598));
#15839=CARTESIAN_POINT('Ctrl Pts',(-5.18994160065279,-3.49569082009585,
7.15948665627275));
#15840=CARTESIAN_POINT('Ctrl Pts',(-5.58406477811046,-3.14370617953113,
7.22985222522876));
#15841=CARTESIAN_POINT('Ctrl Pts',(-6.10419876841606,-3.05543002721108,
7.30007283323036));
#15842=CARTESIAN_POINT('Ctrl Pts',(-6.59085610258569,-3.25712241290123,
7.37019262147636));
#15843=CARTESIAN_POINT('Ctrl Pts',(-6.8952969281062,-3.68642062054244,7.44025632508636));
#15844=CARTESIAN_POINT('Ctrl Pts',(-6.92507910037993,-4.2118623997588,7.51030900497373));
#15845=CARTESIAN_POINT('Ctrl Pts',(-6.67029196164112,-4.6727438878236,7.58039577683535));
#15846=CARTESIAN_POINT('Ctrl Pts',(-6.20902606294958,-4.92782413963266,
7.65056157433059));
#15847=CARTESIAN_POINT('Ctrl Pts',(-5.68175068955988,-4.89838259463549,
7.72085085746158));
#15848=CARTESIAN_POINT('Ctrl Pts',(-5.24995696526907,-4.59224234497362,
7.79130734612191));
#15849=CARTESIAN_POINT('Ctrl Pts',(-5.04653976812282,-4.10189023096155,
7.86197377554524));
#15850=CARTESIAN_POINT('Ctrl Pts',(-5.13553771446182,-3.57654536818086,
7.93289164421975));
#15851=CARTESIAN_POINT('Ctrl Pts',(-5.49167958880606,-3.17757206270347,
8.00410097016463));
#15852=CARTESIAN_POINT('Ctrl Pts',(-6.00820878856796,-3.02820291673281,
8.07564000225066));
#15853=CARTESIAN_POINT('Ctrl Pts',(-6.44062187419601,-3.15261370888403,
8.13556092469148));
#15854=CARTESIAN_POINT('Ctrl Pts',(-6.70861130655355,-3.37965195671477,
8.18369776363854));
#15855=CARTESIAN_POINT('Ctrl Pts',(-6.8937105085998,-3.65581236490976,8.22929135600403));
#15856=CARTESIAN_POINT('Ctrl Pts',(-6.97571459288556,-4.05892831151958,
8.28449961702882));
#15857=CARTESIAN_POINT('Ctrl Pts',(-6.83301647708075,-4.52172879570838,
8.34949564023339));
#15858=CARTESIAN_POINT('Ctrl Pts',(-6.51381452164907,-4.83374162454526,
8.40942447333573));
#15859=CARTESIAN_POINT('Ctrl Pts',(-6.13367096105595,-4.96658596055631,
8.46419547642941));
#15860=CARTESIAN_POINT('Ctrl Pts',(-5.77000769054747,-4.95325944490059,
8.51371979160536));
#15861=CARTESIAN_POINT('Ctrl Pts',(-5.43473421944715,-4.80705755452014,
8.56348049202891));
#15862=CARTESIAN_POINT('Ctrl Pts',(-5.17476962038704,-4.5473411130966,8.6134828902317));
#15863=CARTESIAN_POINT('Ctrl Pts',(-5.02691233865341,-4.20890181210803,
8.66373168353468));
#15864=CARTESIAN_POINT('Ctrl Pts',(-5.01287597198371,-3.83802632501149,
8.71423091550292));
#15865=CARTESIAN_POINT('Ctrl Pts',(-5.13588065841094,-3.48587318149708,
8.76498396862734));
#15866=CARTESIAN_POINT('Ctrl Pts',(-5.38027484984219,-3.20156985271231,
8.81599355960519));
#15867=CARTESIAN_POINT('Ctrl Pts',(-5.71337748308179,-3.0254571982762,8.86726173709343));
#15868=CARTESIAN_POINT('Ctrl Pts',(-6.08966550245643,-2.98274869856715,
8.91878984711541));
#15869=CARTESIAN_POINT('Ctrl Pts',(-6.45733798876018,-3.0812109148485,8.97057858675351));
#15870=CARTESIAN_POINT('Ctrl Pts',(-6.76529910592523,-3.30812336168265,
9.02262792849601));
#15871=CARTESIAN_POINT('Ctrl Pts',(-6.96998046112789,-3.63355675694242,
9.07493719450744));
#15872=CARTESIAN_POINT('Ctrl Pts',(-7.04194989283072,-4.01319995364602,
9.12750500078302));
#15873=CARTESIAN_POINT('Ctrl Pts',(-6.96991048459342,-4.39460760383808,
9.18032929219698));
#15874=CARTESIAN_POINT('Ctrl Pts',(-6.73960211403654,-4.76194359718324,
9.23930488555841));
#15875=CARTESIAN_POINT('Ctrl Pts',(-6.33176853957225,-5.02597941464994,
9.30453505646424));
#15876=CARTESIAN_POINT('Ctrl Pts',(-5.79980377218573,-5.06633098935627,
9.37613051632468));
#15877=CARTESIAN_POINT('Ctrl Pts',(-5.29005475531646,-4.836901018808,9.45115010972279));
#15878=CARTESIAN_POINT('Ctrl Pts',(-4.94827191401131,-4.35650564743655,
9.52964181326016));
#15879=CARTESIAN_POINT('Ctrl Pts',(-4.91327405487842,-3.74129847888372,
9.61164803952703));
#15880=CARTESIAN_POINT('Ctrl Pts',(-5.21254904956895,-3.19880095424663,
9.69412425066449));
#15881=CARTESIAN_POINT('Ctrl Pts',(-5.75755518053287,-2.89705290752891,
9.77704206923956));
#15882=CARTESIAN_POINT('Ctrl Pts',(-6.38261532053777,-2.93174547355756,
9.86037047436186));
#15883=CARTESIAN_POINT('Ctrl Pts',(-6.89571246871018,-3.29533246954376,
9.9440760489684));
#15884=CARTESIAN_POINT('Ctrl Pts',(-7.13766462222267,-3.87856431327716,
10.0281231253342));
#15885=CARTESIAN_POINT('Ctrl Pts',(-7.03181307520858,-4.50336859593469,
10.112474009291));
#15886=CARTESIAN_POINT('Ctrl Pts',(-6.60841405754483,-4.9775421382096,10.1970892234063));
#15887=CARTESIAN_POINT('Ctrl Pts',(-5.99601356400164,-5.15419586953956,
10.2819277209876));
#15888=CARTESIAN_POINT('Ctrl Pts',(-5.38220054085499,-4.97753568370925,
10.3669471364924));
#15889=CARTESIAN_POINT('Ctrl Pts',(-4.95580917322647,-4.50058383383181,
10.4521040148979));
#15890=CARTESIAN_POINT('Ctrl Pts',(-4.84845524689304,-3.86918295104257,
10.5373541217208));
#15891=CARTESIAN_POINT('Ctrl Pts',(-5.09367725879538,-3.27712852401529,
10.6226526455382));
#15892=CARTESIAN_POINT('Ctrl Pts',(-5.6163401918585,-2.90630478068196,10.7079544990261));
#15893=CARTESIAN_POINT('Ctrl Pts',(-6.25592072702474,-2.87046899980689,
10.7932145516894));
#15894=CARTESIAN_POINT('Ctrl Pts',(-6.81586294759382,-3.18009679237689,
10.8783879977619));
#15895=CARTESIAN_POINT('Ctrl Pts',(-7.124955642463,-3.73939634942269,10.963430385322));
#15896=CARTESIAN_POINT('Ctrl Pts',(-7.08867264951758,-4.37593520057008,
11.0482983435205));
#15897=CARTESIAN_POINT('Ctrl Pts',(-6.72062823969146,-4.89450906450982,
11.1329488746335));
#15898=CARTESIAN_POINT('Ctrl Pts',(-6.13472454520284,-5.136799701332,11.217341733611));
#15899=CARTESIAN_POINT('Ctrl Pts',(-5.51200536776972,-5.03087324497862,
11.3014349939178));
#15900=CARTESIAN_POINT('Ctrl Pts',(-5.04306930328679,-4.6109089567958,11.3851957518917));
#15901=CARTESIAN_POINT('Ctrl Pts',(-4.92780437314592,-4.2103503377694,11.4407823887583));
#15902=CARTESIAN_POINT('Ctrl Pts',(-4.92777733020741,-4.00946826990451,
11.4685145081939));
#15903=CARTESIAN_POINT('',(-5.0000018410068,-3.98632452652701,2.60093950625047));
#15904=CARTESIAN_POINT('Origin',(-5.,-4.,2.7));
#15905=CARTESIAN_POINT('',(-4.92777733020741,-4.00946826990451,11.4685145081939));
#15906=CARTESIAN_POINT('Ctrl Pts',(-5.0000018410068,-3.98632452652701,2.60093950625047));
#15907=CARTESIAN_POINT('Ctrl Pts',(-5.00002711936198,-3.79855038268961,
2.62686205390092));
#15908=CARTESIAN_POINT('Ctrl Pts',(-5.10766548646186,-3.42414266353048,
2.67881373981085));
#15909=CARTESIAN_POINT('Ctrl Pts',(-5.54728618664091,-3.02997941177219,
2.75738438838345));
#15910=CARTESIAN_POINT('Ctrl Pts',(-6.13328094577175,-2.93005881251319,
2.83651316903494));
#15911=CARTESIAN_POINT('Ctrl Pts',(-6.68670283260197,-3.15858336118752,
2.91622304878198));
#15912=CARTESIAN_POINT('Ctrl Pts',(-7.03616187921695,-3.65012597802659,
2.99648821676135));
#15913=CARTESIAN_POINT('Ctrl Pts',(-7.07062949516082,-4.25616589762635,
3.07729930317819));
#15914=CARTESIAN_POINT('Ctrl Pts',(-6.77580863517498,-4.79139923899731,
3.15863489698049));
#15915=CARTESIAN_POINT('Ctrl Pts',(-6.23777999713871,-5.08919902934938,
3.24047455745509));
#15916=CARTESIAN_POINT('Ctrl Pts',(-5.62032344264714,-5.05504677509261,
3.32279321070673));
#15917=CARTESIAN_POINT('Ctrl Pts',(-5.11287137916696,-4.69557478020053,
3.40556356877954));
#15918=CARTESIAN_POINT('Ctrl Pts',(-4.87329914702911,-4.11831903637453,
3.48875540125931));
#15919=CARTESIAN_POINT('Ctrl Pts',(-4.97807346419814,-3.49920456570944,
3.57233609900605));
#15920=CARTESIAN_POINT('Ctrl Pts',(-5.39799493781825,-3.02877333945258,
3.65627071903615));
#15921=CARTESIAN_POINT('Ctrl Pts',(-6.00610273172108,-2.85326324045065,
3.74052224127624));
#15922=CARTESIAN_POINT('Ctrl Pts',(-6.61643757836359,-3.02876545098225,
3.82505176791358));
#15923=CARTESIAN_POINT('Ctrl Pts',(-7.02513160270699,-3.48597574268572,
3.90667922493066));
#15924=CARTESIAN_POINT('Ctrl Pts',(-7.12235641775929,-3.9685483460108,3.97275270898905));
#15925=CARTESIAN_POINT('Ctrl Pts',(-7.06636481269846,-4.28466100128236,
4.01685604551847));
#15926=CARTESIAN_POINT('Ctrl Pts',(-7.00182040328561,-4.45530975229043,
4.04207155819959));
#15927=CARTESIAN_POINT('Ctrl Pts',(-6.87402691871924,-4.69744869614318,
4.07990746733096));
#15928=CARTESIAN_POINT('Ctrl Pts',(-6.57124878899927,-4.99309357202046,
4.1367051149187));
#15929=CARTESIAN_POINT('Ctrl Pts',(-6.02768033690931,-5.14605913758532,
4.2124974864954));
#15930=CARTESIAN_POINT('Ctrl Pts',(-5.47679456345111,-5.0204436702095,4.28832048286543));
#15931=CARTESIAN_POINT('Ctrl Pts',(-5.08889541312948,-4.67743201497751,
4.35782392862843));
#15932=CARTESIAN_POINT('Ctrl Pts',(-4.90355272665998,-4.25185719379132,
4.42098501738742));
#15933=CARTESIAN_POINT('Ctrl Pts',(-4.88772422317122,-3.83457870292561,
4.47779828347438));
#15934=CARTESIAN_POINT('Ctrl Pts',(-5.02577825319216,-3.44096047951616,
4.5345666000236));
#15935=CARTESIAN_POINT('Ctrl Pts',(-5.32758243531257,-3.08955719770179,
4.59757801626674));
#15936=CARTESIAN_POINT('Ctrl Pts',(-5.79757132369034,-2.87764760865861,
4.66678930745632));
#15937=CARTESIAN_POINT('Ctrl Pts',(-6.35748141231083,-2.91980778121556,
4.74213608943437));
#15938=CARTESIAN_POINT('Ctrl Pts',(-6.72958410590507,-3.16055362161142,
4.80163845366161));
#15939=CARTESIAN_POINT('Ctrl Pts',(-6.922583408066,-3.41255717151317,4.8453962925926));
#15940=CARTESIAN_POINT('Ctrl Pts',(-7.04520229026909,-3.65506744231538,
4.88286085267916));
#15941=CARTESIAN_POINT('Ctrl Pts',(-7.10903827020174,-3.9926759490213,4.92960885619655));
#15942=CARTESIAN_POINT('Ctrl Pts',(-7.032354492376,-4.39667067923105,4.98556279568034));
#15943=CARTESIAN_POINT('Ctrl Pts',(-6.81415974257675,-4.74396102273289,
5.04136211338037));
#15944=CARTESIAN_POINT('Ctrl Pts',(-6.48510242262688,-4.98648342248571,
5.09699623581333));
#15945=CARTESIAN_POINT('Ctrl Pts',(-6.09122164110091,-5.09213718968761,
5.15245506498449));
#15946=CARTESIAN_POINT('Ctrl Pts',(-5.6879156360413,-5.04618557814476,5.20772889788153));
#15947=CARTESIAN_POINT('Ctrl Pts',(-5.20960410281967,-4.79482820495352,
5.28116853491036));
#15948=CARTESIAN_POINT('Ctrl Pts',(-4.85635661256684,-4.18339627204868,
5.37246079310469));
#15949=CARTESIAN_POINT('Ctrl Pts',(-5.04534497366866,-3.36152922837358,
5.4811368047244));
#15950=CARTESIAN_POINT('Ctrl Pts',(-5.62045222073828,-2.97210695679973,
5.57092649482181));
#15951=CARTESIAN_POINT('Ctrl Pts',(-6.14491401311764,-2.95446524901901,
5.64227218329944));
#15952=CARTESIAN_POINT('Ctrl Pts',(-6.55538629310792,-3.09741218079302,
5.70145206897501));
#15953=CARTESIAN_POINT('Ctrl Pts',(-6.90061904209687,-3.43455608810828,
5.76619150175189));
#15954=CARTESIAN_POINT('Ctrl Pts',(-7.05403180026006,-3.93434682913999,
5.83636208061574));
#15955=CARTESIAN_POINT('Ctrl Pts',(-6.95084370870626,-4.44331194962687,
5.90607316768221));
#15956=CARTESIAN_POINT('Ctrl Pts',(-6.61884201115902,-4.83828819326241,
5.97532164622816));
#15957=CARTESIAN_POINT('Ctrl Pts',(-6.14163977231472,-5.02507153362565,
6.04410658214742));
#15958=CARTESIAN_POINT('Ctrl Pts',(-5.67874308979945,-4.96670943531882,
6.10673565115305));
#15959=CARTESIAN_POINT('Ctrl Pts',(-5.32673727495899,-4.74487796933182,
6.16333654805419));
#15960=CARTESIAN_POINT('Ctrl Pts',(-5.10557737295403,-4.44521639081723,
6.21402149420468));
#15961=CARTESIAN_POINT('Ctrl Pts',(-5.00986236436416,-4.08706033297606,
6.26445344628883));
#15962=CARTESIAN_POINT('Ctrl Pts',(-5.05132140869747,-3.72058500062059,
6.31463598386295));
#15963=CARTESIAN_POINT('Ctrl Pts',(-5.22295427342147,-3.39619318419661,
6.36457331207659));
#15964=CARTESIAN_POINT('Ctrl Pts',(-5.49996349858563,-3.15797332202467,
6.41427030413784));
#15965=CARTESIAN_POINT('Ctrl Pts',(-5.843023257891,-3.03825996963253,6.46373244033231));
#15966=CARTESIAN_POINT('Ctrl Pts',(-6.2651798733637,-3.05368284090179,6.52117143934356));
#15967=CARTESIAN_POINT('Ctrl Pts',(-6.69395218073661,-3.29085487418832,
6.58644589644131));
#15968=CARTESIAN_POINT('Ctrl Pts',(-6.9588514090406,-3.77142724594311,6.65940509135759));
#15969=CARTESIAN_POINT('Ctrl Pts',(-6.93289301903251,-4.22410112506723,
6.71983222544231));
#15970=CARTESIAN_POINT('Ctrl Pts',(-6.77106481048377,-4.53615877260298,
6.76796591761938));
#15971=CARTESIAN_POINT('Ctrl Pts',(-6.57088599598262,-4.74749645053629,
6.8079662999785));
#15972=CARTESIAN_POINT('Ctrl Pts',(-6.18196007039062,-4.95496402481898,
6.86778079666891));
#15973=CARTESIAN_POINT('Ctrl Pts',(-5.63200940413013,-4.91297894303413,
6.93919834468442));
#15974=CARTESIAN_POINT('Ctrl Pts',(-5.18963313111942,-4.51545599119052,
7.01814869825501));
#15975=CARTESIAN_POINT('Ctrl Pts',(-5.04266994609727,-4.00519996765647,
7.08893288548598));
#15976=CARTESIAN_POINT('Ctrl Pts',(-5.18994160065279,-3.49569082009585,
7.15948665627275));
#15977=CARTESIAN_POINT('Ctrl Pts',(-5.58406477811046,-3.14370617953113,
7.22985222522876));
#15978=CARTESIAN_POINT('Ctrl Pts',(-6.10419876841606,-3.05543002721108,
7.30007283323036));
#15979=CARTESIAN_POINT('Ctrl Pts',(-6.59085610258569,-3.25712241290123,
7.37019262147636));
#15980=CARTESIAN_POINT('Ctrl Pts',(-6.8952969281062,-3.68642062054244,7.44025632508636));
#15981=CARTESIAN_POINT('Ctrl Pts',(-6.92507910037993,-4.2118623997588,7.51030900497373));
#15982=CARTESIAN_POINT('Ctrl Pts',(-6.67029196164112,-4.6727438878236,7.58039577683535));
#15983=CARTESIAN_POINT('Ctrl Pts',(-6.20902606294958,-4.92782413963266,
7.65056157433059));
#15984=CARTESIAN_POINT('Ctrl Pts',(-5.68175068955988,-4.89838259463549,
7.72085085746158));
#15985=CARTESIAN_POINT('Ctrl Pts',(-5.24995696526907,-4.59224234497362,
7.79130734612191));
#15986=CARTESIAN_POINT('Ctrl Pts',(-5.04653976812282,-4.10189023096155,
7.86197377554524));
#15987=CARTESIAN_POINT('Ctrl Pts',(-5.13553771446182,-3.57654536818086,
7.93289164421975));
#15988=CARTESIAN_POINT('Ctrl Pts',(-5.49167958880606,-3.17757206270347,
8.00410097016463));
#15989=CARTESIAN_POINT('Ctrl Pts',(-6.00820878856796,-3.02820291673281,
8.07564000225066));
#15990=CARTESIAN_POINT('Ctrl Pts',(-6.44062187419601,-3.15261370888403,
8.13556092469148));
#15991=CARTESIAN_POINT('Ctrl Pts',(-6.70861130655355,-3.37965195671477,
8.18369776363854));
#15992=CARTESIAN_POINT('Ctrl Pts',(-6.8937105085998,-3.65581236490976,8.22929135600403));
#15993=CARTESIAN_POINT('Ctrl Pts',(-6.97571459288556,-4.05892831151958,
8.28449961702882));
#15994=CARTESIAN_POINT('Ctrl Pts',(-6.83301647708075,-4.52172879570838,
8.34949564023339));
#15995=CARTESIAN_POINT('Ctrl Pts',(-6.51381452164907,-4.83374162454526,
8.40942447333573));
#15996=CARTESIAN_POINT('Ctrl Pts',(-6.13367096105595,-4.96658596055631,
8.46419547642941));
#15997=CARTESIAN_POINT('Ctrl Pts',(-5.77000769054747,-4.95325944490059,
8.51371979160536));
#15998=CARTESIAN_POINT('Ctrl Pts',(-5.43473421944715,-4.80705755452014,
8.56348049202891));
#15999=CARTESIAN_POINT('Ctrl Pts',(-5.17476962038704,-4.5473411130966,8.6134828902317));
#16000=CARTESIAN_POINT('Ctrl Pts',(-5.02691233865341,-4.20890181210803,
8.66373168353468));
#16001=CARTESIAN_POINT('Ctrl Pts',(-5.01287597198371,-3.83802632501149,
8.71423091550292));
#16002=CARTESIAN_POINT('Ctrl Pts',(-5.13588065841094,-3.48587318149708,
8.76498396862734));
#16003=CARTESIAN_POINT('Ctrl Pts',(-5.38027484984219,-3.20156985271231,
8.81599355960519));
#16004=CARTESIAN_POINT('Ctrl Pts',(-5.71337748308179,-3.0254571982762,8.86726173709343));
#16005=CARTESIAN_POINT('Ctrl Pts',(-6.08966550245643,-2.98274869856715,
8.91878984711541));
#16006=CARTESIAN_POINT('Ctrl Pts',(-6.45733798876018,-3.0812109148485,8.97057858675351));
#16007=CARTESIAN_POINT('Ctrl Pts',(-6.76529910592523,-3.30812336168265,
9.02262792849601));
#16008=CARTESIAN_POINT('Ctrl Pts',(-6.96998046112789,-3.63355675694242,
9.07493719450744));
#16009=CARTESIAN_POINT('Ctrl Pts',(-7.04194989283072,-4.01319995364602,
9.12750500078302));
#16010=CARTESIAN_POINT('Ctrl Pts',(-6.96991048459342,-4.39460760383808,
9.18032929219698));
#16011=CARTESIAN_POINT('Ctrl Pts',(-6.73960211403654,-4.76194359718324,
9.23930488555841));
#16012=CARTESIAN_POINT('Ctrl Pts',(-6.33176853957225,-5.02597941464994,
9.30453505646424));
#16013=CARTESIAN_POINT('Ctrl Pts',(-5.79980377218573,-5.06633098935627,
9.37613051632468));
#16014=CARTESIAN_POINT('Ctrl Pts',(-5.29005475531646,-4.836901018808,9.45115010972279));
#16015=CARTESIAN_POINT('Ctrl Pts',(-4.94827191401131,-4.35650564743655,
9.52964181326016));
#16016=CARTESIAN_POINT('Ctrl Pts',(-4.91327405487842,-3.74129847888372,
9.61164803952703));
#16017=CARTESIAN_POINT('Ctrl Pts',(-5.21254904956895,-3.19880095424663,
9.69412425066449));
#16018=CARTESIAN_POINT('Ctrl Pts',(-5.75755518053287,-2.89705290752891,
9.77704206923956));
#16019=CARTESIAN_POINT('Ctrl Pts',(-6.38261532053777,-2.93174547355756,
9.86037047436186));
#16020=CARTESIAN_POINT('Ctrl Pts',(-6.89571246871018,-3.29533246954376,
9.9440760489684));
#16021=CARTESIAN_POINT('Ctrl Pts',(-7.13766462222267,-3.87856431327716,
10.0281231253342));
#16022=CARTESIAN_POINT('Ctrl Pts',(-7.03181307520858,-4.50336859593469,
10.112474009291));
#16023=CARTESIAN_POINT('Ctrl Pts',(-6.60841405754483,-4.9775421382096,10.1970892234063));
#16024=CARTESIAN_POINT('Ctrl Pts',(-5.99601356400164,-5.15419586953956,
10.2819277209876));
#16025=CARTESIAN_POINT('Ctrl Pts',(-5.38220054085499,-4.97753568370925,
10.3669471364924));
#16026=CARTESIAN_POINT('Ctrl Pts',(-4.95580917322647,-4.50058383383181,
10.4521040148979));
#16027=CARTESIAN_POINT('Ctrl Pts',(-4.84845524689304,-3.86918295104257,
10.5373541217208));
#16028=CARTESIAN_POINT('Ctrl Pts',(-5.09367725879538,-3.27712852401529,
10.6226526455382));
#16029=CARTESIAN_POINT('Ctrl Pts',(-5.6163401918585,-2.90630478068196,10.7079544990261));
#16030=CARTESIAN_POINT('Ctrl Pts',(-6.25592072702474,-2.87046899980689,
10.7932145516894));
#16031=CARTESIAN_POINT('Ctrl Pts',(-6.81586294759382,-3.18009679237689,
10.8783879977619));
#16032=CARTESIAN_POINT('Ctrl Pts',(-7.124955642463,-3.73939634942269,10.963430385322));
#16033=CARTESIAN_POINT('Ctrl Pts',(-7.08867264951758,-4.37593520057008,
11.0482983435205));
#16034=CARTESIAN_POINT('Ctrl Pts',(-6.72062823969146,-4.89450906450982,
11.1329488746335));
#16035=CARTESIAN_POINT('Ctrl Pts',(-6.13472454520284,-5.136799701332,11.217341733611));
#16036=CARTESIAN_POINT('Ctrl Pts',(-5.51200536776972,-5.03087324497862,
11.3014349939178));
#16037=CARTESIAN_POINT('Ctrl Pts',(-5.04306930328679,-4.6109089567958,11.3851957518917));
#16038=CARTESIAN_POINT('Ctrl Pts',(-4.92780437314592,-4.2103503377694,11.4407823887583));
#16039=CARTESIAN_POINT('Ctrl Pts',(-4.92777733020741,-4.00946826990451,
11.4685145081939));
#16040=CARTESIAN_POINT('Origin',(-5.,-4.,11.4));
#16041=CARTESIAN_POINT('Origin',(-5.,-4.,11.4));
#16042=CARTESIAN_POINT('Origin',(-5.,-4.,2.7));
#16043=CARTESIAN_POINT('',(0.,0.,0.));
#16044=CARTESIAN_POINT('Origin',(-7.6,6.7,-0.1));
#16045=CARTESIAN_POINT('',(-7.81,6.7,0.));
#16046=CARTESIAN_POINT('Origin',(-7.6,6.7,0.));
#16047=CARTESIAN_POINT('',(-7.81,6.7,0.9));
#16048=CARTESIAN_POINT('',(-7.81,6.7,-0.1));
#16049=CARTESIAN_POINT('Origin',(-7.6,6.7,0.9));
#16050=CARTESIAN_POINT('Origin',(-7.6,6.7,0.9));
#16051=CARTESIAN_POINT('Origin',(-4.4,6.7,-0.1));
#16052=CARTESIAN_POINT('',(-4.61,6.7,0.));
#16053=CARTESIAN_POINT('Origin',(-4.4,6.7,0.));
#16054=CARTESIAN_POINT('',(-4.61,6.7,0.9));
#16055=CARTESIAN_POINT('',(-4.61,6.7,-0.1));
#16056=CARTESIAN_POINT('Origin',(-4.4,6.7,0.9));
#16057=CARTESIAN_POINT('Origin',(-4.4,6.7,0.9));
#16058=CARTESIAN_POINT('Origin',(-7.6,6.2,1.2));
#16059=CARTESIAN_POINT('',(-7.81,6.3,1.2));
#16060=CARTESIAN_POINT('Origin',(-7.6,6.3,1.2));
#16061=CARTESIAN_POINT('',(-7.81,7.1,1.2));
#16062=CARTESIAN_POINT('',(-7.81,6.2,1.2));
#16063=CARTESIAN_POINT('Origin',(-7.6,7.1,1.2));
#16064=CARTESIAN_POINT('Origin',(-4.4,6.2,1.2));
#16065=CARTESIAN_POINT('',(-4.61,6.3,1.2));
#16066=CARTESIAN_POINT('Origin',(-4.4,6.3,1.2));
#16067=CARTESIAN_POINT('',(-4.61,7.1,1.2));
#16068=CARTESIAN_POINT('',(-4.61,6.2,1.2));
#16069=CARTESIAN_POINT('Origin',(-4.4,7.1,1.2));
#16070=CARTESIAN_POINT('Origin',(-3.6,7.1,0.));
#16071=CARTESIAN_POINT('',(-3.6,7.1,0.));
#16072=CARTESIAN_POINT('',(-8.4,7.1,0.));
#16073=CARTESIAN_POINT('',(-3.6,7.1,0.));
#16074=CARTESIAN_POINT('',(-8.4,7.1,3.));
#16075=CARTESIAN_POINT('',(-8.4,7.1,0.));
#16076=CARTESIAN_POINT('',(-3.6,7.1,3.));
#16077=CARTESIAN_POINT('',(-3.6,7.1,3.));
#16078=CARTESIAN_POINT('',(-3.6,7.1,0.));
#16079=CARTESIAN_POINT('Origin',(-3.6,6.3,0.));
#16080=CARTESIAN_POINT('',(-3.6,6.3,0.));
#16081=CARTESIAN_POINT('',(-3.6,6.3,0.));
#16082=CARTESIAN_POINT('',(-3.6,6.3,3.));
#16083=CARTESIAN_POINT('',(-3.6,6.3,3.));
#16084=CARTESIAN_POINT('',(-3.6,6.3,0.));
#16085=CARTESIAN_POINT('Origin',(-8.4,6.3,0.));
#16086=CARTESIAN_POINT('',(-8.4,6.3,0.));
#16087=CARTESIAN_POINT('',(-8.4,6.3,0.));
#16088=CARTESIAN_POINT('',(-8.4,6.3,3.));
#16089=CARTESIAN_POINT('',(-8.4,6.3,3.));
#16090=CARTESIAN_POINT('',(-8.4,6.3,0.));
#16091=CARTESIAN_POINT('Origin',(-8.4,7.1,0.));
#16092=CARTESIAN_POINT('',(-8.4,7.1,0.));
#16093=CARTESIAN_POINT('',(-8.4,7.1,3.));
#16094=CARTESIAN_POINT('Origin',(-6.,6.7,3.));
#16095=CARTESIAN_POINT('Origin',(-6.,6.7,0.));
#16096=CARTESIAN_POINT('',(0.,0.,0.));
#16097=CARTESIAN_POINT('Origin',(-7.6,8.,29.6));
#16098=CARTESIAN_POINT('',(-7.81,8.,29.7));
#16099=CARTESIAN_POINT('Origin',(-7.6,8.,29.7));
#16100=CARTESIAN_POINT('',(-7.81,8.,30.5));
#16101=CARTESIAN_POINT('',(-7.81,8.,29.6));
#16102=CARTESIAN_POINT('Origin',(-7.6,8.,30.5));
#16103=CARTESIAN_POINT('Origin',(-4.4,8.,29.6));
#16104=CARTESIAN_POINT('',(-4.61,8.,29.7));
#16105=CARTESIAN_POINT('Origin',(-4.4,8.,29.7));
#16106=CARTESIAN_POINT('',(-4.61,8.,30.5));
#16107=CARTESIAN_POINT('',(-4.61,8.,29.6));
#16108=CARTESIAN_POINT('Origin',(-4.4,8.,30.5));
#16109=CARTESIAN_POINT('Origin',(-7.6,6.2,29.8));
#16110=CARTESIAN_POINT('',(-7.81,6.3,29.8));
#16111=CARTESIAN_POINT('Origin',(-7.6,6.3,29.8));
#16112=CARTESIAN_POINT('',(-7.81,7.2,29.8));
#16113=CARTESIAN_POINT('',(-7.81,6.2,29.8));
#16114=CARTESIAN_POINT('',(-7.41533814687381,7.2,29.7));
#16115=CARTESIAN_POINT('Origin',(-7.6,7.2,29.8));
#16116=CARTESIAN_POINT('',(-7.4153381468738,7.1,29.7));
#16117=CARTESIAN_POINT('',(-7.41533814687381,6.2,29.7));
#16118=CARTESIAN_POINT('',(-7.78466185312619,7.1,29.7));
#16119=CARTESIAN_POINT('Origin',(-7.6,7.1,29.8));
#16120=CARTESIAN_POINT('',(-7.78466185312619,7.2,29.7));
#16121=CARTESIAN_POINT('',(-7.78466185312619,6.2,29.7));
#16122=CARTESIAN_POINT('Origin',(-7.6,7.2,29.8));
#16123=CARTESIAN_POINT('Origin',(-7.6,7.2,29.8));
#16124=CARTESIAN_POINT('',(-5.6,7.2,29.7));
#16125=CARTESIAN_POINT('Origin',(-4.4,6.2,29.8));
#16126=CARTESIAN_POINT('',(-4.61,6.3,29.8));
#16127=CARTESIAN_POINT('Origin',(-4.4,6.3,29.8));
#16128=CARTESIAN_POINT('',(-4.61,7.2,29.8));
#16129=CARTESIAN_POINT('',(-4.61,6.2,29.8));
#16130=CARTESIAN_POINT('',(-4.21533814687381,7.2,29.7));
#16131=CARTESIAN_POINT('Origin',(-4.4,7.2,29.8));
#16132=CARTESIAN_POINT('',(-4.21533814687381,7.1,29.7));
#16133=CARTESIAN_POINT('',(-4.21533814687381,6.2,29.7));
#16134=CARTESIAN_POINT('',(-4.5846618531262,7.1,29.7));
#16135=CARTESIAN_POINT('Origin',(-4.4,7.1,29.8));
#16136=CARTESIAN_POINT('',(-4.58466185312619,7.2,29.7));
#16137=CARTESIAN_POINT('',(-4.58466185312619,6.2,29.7));
#16138=CARTESIAN_POINT('Origin',(-4.4,7.2,29.8));
#16139=CARTESIAN_POINT('Origin',(-4.4,7.2,29.8));
#16140=CARTESIAN_POINT('',(-4.,7.2,29.7));
#16141=CARTESIAN_POINT('Origin',(-3.6,7.1,28.));
#16142=CARTESIAN_POINT('',(-3.6,7.1,29.7));
#16143=CARTESIAN_POINT('',(-3.6,7.1,29.7));
#16144=CARTESIAN_POINT('',(-3.6,7.1,29.7));
#16145=CARTESIAN_POINT('',(-3.6,7.1,28.));
#16146=CARTESIAN_POINT('',(-3.6,7.1,28.));
#16147=CARTESIAN_POINT('',(-8.4,7.1,28.));
#16148=CARTESIAN_POINT('',(-3.6,7.1,28.));
#16149=CARTESIAN_POINT('',(-8.4,7.1,29.7));
#16150=CARTESIAN_POINT('',(-8.4,7.1,28.));
#16151=CARTESIAN_POINT('',(-3.6,7.1,29.7));
#16152=CARTESIAN_POINT('Origin',(-3.6,6.3,29.7));
#16153=CARTESIAN_POINT('',(-8.4,9.,29.7));
#16154=CARTESIAN_POINT('',(-8.4,6.3,29.7));
#16155=CARTESIAN_POINT('',(-3.6,9.,29.7));
#16156=CARTESIAN_POINT('',(-8.4,9.,29.7));
#16157=CARTESIAN_POINT('',(-3.6,6.3,29.7));
#16158=CARTESIAN_POINT('Origin',(-6.,9.,30.1));
#16159=CARTESIAN_POINT('',(-8.4,9.,30.5));
#16160=CARTESIAN_POINT('',(-3.6,9.,30.5));
#16161=CARTESIAN_POINT('',(-3.6,9.,30.5));
#16162=CARTESIAN_POINT('',(-3.6,9.,29.7));
#16163=CARTESIAN_POINT('',(-8.4,9.,30.5));
#16164=CARTESIAN_POINT('Origin',(-3.6,6.3,28.));
#16165=CARTESIAN_POINT('',(-3.6,6.3,28.));
#16166=CARTESIAN_POINT('',(-3.6,6.3,30.5));
#16167=CARTESIAN_POINT('',(-3.6,6.3,28.));
#16168=CARTESIAN_POINT('',(-3.6,6.3,28.));
#16169=CARTESIAN_POINT('',(-3.6,6.3,30.5));
#16170=CARTESIAN_POINT('Origin',(-8.4,6.3,28.));
#16171=CARTESIAN_POINT('',(-8.4,6.3,28.));
#16172=CARTESIAN_POINT('',(-8.4,6.3,30.5));
#16173=CARTESIAN_POINT('',(-8.4,6.3,28.));
#16174=CARTESIAN_POINT('',(-8.4,6.3,28.));
#16175=CARTESIAN_POINT('',(-8.4,6.3,30.5));
#16176=CARTESIAN_POINT('Origin',(-8.4,7.1,28.));
#16177=CARTESIAN_POINT('',(-8.4,7.1,28.));
#16178=CARTESIAN_POINT('',(-8.4,6.3,30.5));
#16179=CARTESIAN_POINT('Origin',(-6.,6.7,30.5));
#16180=CARTESIAN_POINT('Origin',(-6.,6.7,28.));
#16181=CARTESIAN_POINT('',(0.,0.,0.));
#16182=CARTESIAN_POINT('Origin',(-6.,4.,1.9));
#16183=CARTESIAN_POINT('',(-6.625,4.,2.6));
#16184=CARTESIAN_POINT('Origin',(-6.,4.,2.6));
#16185=CARTESIAN_POINT('',(-6.625,4.,1.9));
#16186=CARTESIAN_POINT('',(-6.625,4.,1.9));
#16187=CARTESIAN_POINT('Origin',(-6.,4.,1.9));
#16188=CARTESIAN_POINT('Origin',(-6.,4.,1.9));
#16189=CARTESIAN_POINT('',(-7.5,4.,2.6));
#16190=CARTESIAN_POINT('Origin',(-6.,4.,2.6));
#16191=CARTESIAN_POINT('',(-7.5,4.,1.9));
#16192=CARTESIAN_POINT('',(-7.5,4.,1.9));
#16193=CARTESIAN_POINT('Origin',(-6.,4.,1.9));
#16194=CARTESIAN_POINT('Origin',(-6.,4.,2.6));
#16195=CARTESIAN_POINT('Origin',(-6.,4.,1.9));
#16196=CARTESIAN_POINT('',(0.,0.,0.));
#16197=CARTESIAN_POINT('Ctrl Pts',(-5.00000184100681,4.0136754734751,2.60093950625076));
#16198=CARTESIAN_POINT('Ctrl Pts',(-5.00002711936209,4.20144961727963,2.62686205390075));
#16199=CARTESIAN_POINT('Ctrl Pts',(-5.1076914443916,4.57620101292901,2.67882571929646));
#16200=CARTESIAN_POINT('Ctrl Pts',(-5.54731085839696,4.97011855968613,2.75738770095752));
#16201=CARTESIAN_POINT('Ctrl Pts',(-6.13330829028169,5.07009398433603,2.83651804650349));
#16202=CARTESIAN_POINT('Ctrl Pts',(-6.68676060294283,4.84148936906199,2.91622569034364));
#16203=CARTESIAN_POINT('Ctrl Pts',(-7.03617542740839,4.34995411926946,2.99649057036664));
#16204=CARTESIAN_POINT('Ctrl Pts',(-7.07077171566156,3.74380977688242,3.07730075350998));
#16205=CARTESIAN_POINT('Ctrl Pts',(-6.77566001133407,3.20870450421941,3.15863603264667));
#16206=CARTESIAN_POINT('Ctrl Pts',(-6.23777975703619,2.91082274760045,3.24047540010177));
#16207=CARTESIAN_POINT('Ctrl Pts',(-5.62027751939497,2.94499359194798,3.32279385402167));
#16208=CARTESIAN_POINT('Ctrl Pts',(-5.1128578559771,3.30444603110391,3.40556404882598));
#16209=CARTESIAN_POINT('Ctrl Pts',(-4.87328209631149,3.88170381609706,3.48875576249667));
#16210=CARTESIAN_POINT('Ctrl Pts',(-4.97806047014568,4.50081578134862,3.57233636795591));
#16211=CARTESIAN_POINT('Ctrl Pts',(-5.39799694068156,4.97124635132397,3.65627091939543));
#16212=CARTESIAN_POINT('Ctrl Pts',(-6.00608186722498,5.1467635917961,3.7405223892875));
#16213=CARTESIAN_POINT('Ctrl Pts',(-6.61648592829516,4.97125245378467,3.82505187703477));
#16214=CARTESIAN_POINT('Ctrl Pts',(-7.02504723026834,4.51407458863333,3.90667930466183));
#16215=CARTESIAN_POINT('Ctrl Pts',(-7.14109507248108,3.93953170138583,3.98533819578826));
#16216=CARTESIAN_POINT('Ctrl Pts',(-6.97515546374893,3.40104443225745,4.06097495793453));
#16217=CARTESIAN_POINT('Ctrl Pts',(-6.57122653386479,3.00706128325563,4.13670514732847));
#16218=CARTESIAN_POINT('Ctrl Pts',(-6.02775857632327,2.85377271371871,4.21249751130402));
#16219=CARTESIAN_POINT('Ctrl Pts',(-5.47693199324532,2.97976879840739,4.28832050275612));
#16220=CARTESIAN_POINT('Ctrl Pts',(-5.08889329636147,3.32248782371839,4.35782394322737));
#16221=CARTESIAN_POINT('Ctrl Pts',(-4.90348334427995,3.74815768282725,4.42098503121462));
#16222=CARTESIAN_POINT('Ctrl Pts',(-4.88777846541416,4.16541417756998,4.47779829335302));
#16223=CARTESIAN_POINT('Ctrl Pts',(-5.02572337488508,4.5591407782775,4.53456660974454));
#16224=CARTESIAN_POINT('Ctrl Pts',(-5.32762081329308,4.91046292297288,4.59757802398128));
#16225=CARTESIAN_POINT('Ctrl Pts',(-5.79769987729577,5.12240617534609,4.6667893141555));
#16226=CARTESIAN_POINT('Ctrl Pts',(-6.35744977854988,5.0800953582818,4.74213609062164));
#16227=CARTESIAN_POINT('Ctrl Pts',(-6.7886388886812,4.80135715932747,4.81103357029135));
#16228=CARTESIAN_POINT('Ctrl Pts',(-7.03217914396847,4.41239214657722,4.87351124701705));
#16229=CARTESIAN_POINT('Ctrl Pts',(-7.13592863330475,3.87207852021905,4.94830807653976));
#16230=CARTESIAN_POINT('Ctrl Pts',(-6.87284718079957,3.20107467373212,5.04144479366485));
#16231=CARTESIAN_POINT('Ctrl Pts',(-6.09623481157017,2.82823992504595,5.15254762809713));
#16232=CARTESIAN_POINT('Ctrl Pts',(-5.27971004197149,3.08146490109176,5.26291010705797));
#16233=CARTESIAN_POINT('Ctrl Pts',(-4.85635349881296,3.81715131471987,5.37246078991772));
#16234=CARTESIAN_POINT('Ctrl Pts',(-5.04487949063783,4.63769677411038,5.48113679376609));
#16235=CARTESIAN_POINT('Ctrl Pts',(-5.73589746055469,5.10693196272956,5.58888446285182));
#16236=CARTESIAN_POINT('Ctrl Pts',(-6.37118793757295,5.00949360744693,5.67193196549858));
#16237=CARTESIAN_POINT('Ctrl Pts',(-6.71254361053678,4.74926813559046,5.73087908447486));
#16238=CARTESIAN_POINT('Ctrl Pts',(-6.92618421314144,4.48213635150675,5.77788659686335));
#16239=CARTESIAN_POINT('Ctrl Pts',(-7.05447791083229,4.06557532936466,5.83636209009091));
#16240=CARTESIAN_POINT('Ctrl Pts',(-6.95088091422359,3.55670409484484,5.90607316301112));
#16241=CARTESIAN_POINT('Ctrl Pts',(-6.61900788359635,3.16160526086392,5.97532164754671));
#16242=CARTESIAN_POINT('Ctrl Pts',(-6.14183402203666,2.97493714351951,6.0441065734333));
#16243=CARTESIAN_POINT('Ctrl Pts',(-5.67880942079896,3.03347123408109,6.10673564359386));
#16244=CARTESIAN_POINT('Ctrl Pts',(-5.32735160410172,3.25520230218429,6.16333652454754));
#16245=CARTESIAN_POINT('Ctrl Pts',(-5.03108251682038,3.65479384285351,6.23091649770626));
#16246=CARTESIAN_POINT('Ctrl Pts',(-4.99209121035488,4.17131828916311,6.29799027327816));
#16247=CARTESIAN_POINT('Ctrl Pts',(-5.22308647377139,4.60388582873653,6.36457330678434));
#16248=CARTESIAN_POINT('Ctrl Pts',(-5.49945070307415,4.84205518395227,6.4142703184249));
#16249=CARTESIAN_POINT('Ctrl Pts',(-5.8429108649416,4.96183684549319,6.46373244635463));
#16250=CARTESIAN_POINT('Ctrl Pts',(-6.26484181971828,4.94625056066266,6.52117144061682));
#16251=CARTESIAN_POINT('Ctrl Pts',(-6.69390577408147,4.70907736638303,6.58644589945804));
#16252=CARTESIAN_POINT('Ctrl Pts',(-6.95873462103172,4.22881797506906,6.65940509116432));
#16253=CARTESIAN_POINT('Ctrl Pts',(-6.93269246532923,3.77588585116234,6.71983222414211));
#16254=CARTESIAN_POINT('Ctrl Pts',(-6.77107468324783,3.46412923688142,6.7679659145118));
#16255=CARTESIAN_POINT('Ctrl Pts',(-6.57079871082626,3.25210408080074,6.80796630929164));
#16256=CARTESIAN_POINT('Ctrl Pts',(-6.28566327773964,3.10148204150563,6.85183024182226));
#16257=CARTESIAN_POINT('Ctrl Pts',(-5.9374350403567,3.06238692304077,6.89952195896654));
#16258=CARTESIAN_POINT('Ctrl Pts',(-5.54350254185785,3.16770824417749,6.95498839067594));
#16259=CARTESIAN_POINT('Ctrl Pts',(-5.18977130243312,3.48372162057587,7.01814871426604));
#16260=CARTESIAN_POINT('Ctrl Pts',(-5.04285761799324,3.99497433346206,7.0889328817521));
#16261=CARTESIAN_POINT('Ctrl Pts',(-5.18978309684873,4.50416337482064,7.15948666242575));
#16262=CARTESIAN_POINT('Ctrl Pts',(-5.58408091231752,4.85632154197909,7.22985222665258));
#16263=CARTESIAN_POINT('Ctrl Pts',(-6.10418851591415,4.94454356395432,7.30007283487924));
#16264=CARTESIAN_POINT('Ctrl Pts',(-6.59084588507658,4.74288104801731,7.37019262264957));
#16265=CARTESIAN_POINT('Ctrl Pts',(-6.89540829263521,4.31357351131412,7.44025632549589));
#16266=CARTESIAN_POINT('Ctrl Pts',(-6.92492923689232,3.78812028153619,7.51030900574892));
#16267=CARTESIAN_POINT('Ctrl Pts',(-6.67028427013333,3.32725098620657,7.58039577698737));
#16268=CARTESIAN_POINT('Ctrl Pts',(-6.20897623341015,3.0721729365591,7.65056157443552));
#16269=CARTESIAN_POINT('Ctrl Pts',(-5.68173783558839,3.10162769981329,7.72085085716389));
#16270=CARTESIAN_POINT('Ctrl Pts',(-5.24992919279951,3.40776503869049,7.79130734597953));
#16271=CARTESIAN_POINT('Ctrl Pts',(-5.0465424843122,3.89815513625059,7.86197377424775));
#16272=CARTESIAN_POINT('Ctrl Pts',(-5.13549244911485,4.42345796985394,7.9328916443029));
#16273=CARTESIAN_POINT('Ctrl Pts',(-5.49174629490197,4.82258141736487,8.00410096577713));
#16274=CARTESIAN_POINT('Ctrl Pts',(-6.00803868168598,4.97171279548103,8.07564000534741));
#16275=CARTESIAN_POINT('Ctrl Pts',(-6.52735154266829,4.82257974695955,8.1475451059773));
#16276=CARTESIAN_POINT('Ctrl Pts',(-6.87597910605558,4.43277936154282,8.2171724616343));
#16277=CARTESIAN_POINT('Ctrl Pts',(-6.97565473561711,3.94102818366579,8.28449961898768));
#16278=CARTESIAN_POINT('Ctrl Pts',(-6.8330580514463,3.47827883486752,8.34949563910535));
#16279=CARTESIAN_POINT('Ctrl Pts',(-6.51380412257741,3.1662390255362,8.40942447363317));
#16280=CARTESIAN_POINT('Ctrl Pts',(-6.13368043091516,3.03340218960474,8.46419547601407));
#16281=CARTESIAN_POINT('Ctrl Pts',(-5.77000963425156,3.04672415558585,8.51371979129401));
#16282=CARTESIAN_POINT('Ctrl Pts',(-5.43474033823938,3.19292650787483,8.56348049163152));
#16283=CARTESIAN_POINT('Ctrl Pts',(-5.17477216956946,3.45264130135924,8.61348288970698));
#16284=CARTESIAN_POINT('Ctrl Pts',(-5.02692180394174,3.79107624660051,8.6637316830418));
#16285=CARTESIAN_POINT('Ctrl Pts',(-5.012872576251,4.16195256384123,8.7142309145088));
#16286=CARTESIAN_POINT('Ctrl Pts',(-5.13590369868626,4.51409239039593,8.76498396821864));
#16287=CARTESIAN_POINT('Ctrl Pts',(-5.38031427946466,4.79836661872066,8.81599356007185));
#16288=CARTESIAN_POINT('Ctrl Pts',(-5.71336668770006,4.97458793379134,8.86726173279411));
#16289=CARTESIAN_POINT('Ctrl Pts',(-6.08968356313292,5.01715924274108,8.918789847283));
#16290=CARTESIAN_POINT('Ctrl Pts',(-6.45738481100365,4.91881570416212,8.9705785818587));
#16291=CARTESIAN_POINT('Ctrl Pts',(-6.76530671813857,4.69177684003305,9.02262792715958));
#16292=CARTESIAN_POINT('Ctrl Pts',(-6.96997065785482,4.36635789720065,9.07493719271063));
#16293=CARTESIAN_POINT('Ctrl Pts',(-7.04206467317586,3.98670152421777,9.12750499448518));
#16294=CARTESIAN_POINT('Ctrl Pts',(-6.96988775131722,3.60530323601265,9.18032928987629));
#16295=CARTESIAN_POINT('Ctrl Pts',(-6.7397150976367,3.23792225540337,9.23930487839808));
#16296=CARTESIAN_POINT('Ctrl Pts',(-6.33166237507248,2.97390330552954,9.30453505300732));
#16297=CARTESIAN_POINT('Ctrl Pts',(-5.79979171434613,2.93396143628525,9.37613052323128));
#16298=CARTESIAN_POINT('Ctrl Pts',(-5.29001663621426,3.16323503239153,9.45115011122364));
#16299=CARTESIAN_POINT('Ctrl Pts',(-4.94825545210904,3.64363042187255,9.52964181259955));
#16300=CARTESIAN_POINT('Ctrl Pts',(-4.91325516498484,4.25878443889604,9.61164803507556));
#16301=CARTESIAN_POINT('Ctrl Pts',(-5.2125378502354,4.80126773521892,9.69412424268727));
#16302=CARTESIAN_POINT('Ctrl Pts',(-5.75754644935023,5.10299443985526,9.77704205666351));
#16303=CARTESIAN_POINT('Ctrl Pts',(-6.38261067907029,5.06829058753974,9.86037045595682));
#16304=CARTESIAN_POINT('Ctrl Pts',(-6.89571009340608,4.70469230712254,9.94407602284259));
#16305=CARTESIAN_POINT('Ctrl Pts',(-7.13766387710299,4.12145232028498,10.0281230888647));
#16306=CARTESIAN_POINT('Ctrl Pts',(-7.03181245317105,3.49664097659948,10.112473958668));
#16307=CARTESIAN_POINT('Ctrl Pts',(-6.60841264630813,3.02246212675956,10.1970891533592));
#16308=CARTESIAN_POINT('Ctrl Pts',(-5.99601006835875,2.8458044826624,10.2819276244449));
#16309=CARTESIAN_POINT('Ctrl Pts',(-5.38219522105592,3.02246199100347,10.3669470032346));
#16310=CARTESIAN_POINT('Ctrl Pts',(-4.95579995827654,3.49941222674329,10.452103831618));
#16311=CARTESIAN_POINT('Ctrl Pts',(-4.84844583817861,4.13081136700949,10.5373538681711));
#16312=CARTESIAN_POINT('Ctrl Pts',(-5.0936581339001,4.72286468788687,10.6226522983686));
#16313=CARTESIAN_POINT('Ctrl Pts',(-5.61632959368519,5.09368411438882,10.7079540155997));
#16314=CARTESIAN_POINT('Ctrl Pts',(-6.25587144748665,5.12951914158568,10.7932138961696));
#16315=CARTESIAN_POINT('Ctrl Pts',(-6.81586867421465,4.81987787722662,10.8783870694892));
#16316=CARTESIAN_POINT('Ctrl Pts',(-7.12478685219004,4.26058878480156,10.9634291596385));
#16317=CARTESIAN_POINT('Ctrl Pts',(-7.08884111245123,3.62399110135786,11.0482965343607));
#16318=CARTESIAN_POINT('Ctrl Pts',(-6.72064073263906,3.10540887765364,11.132946666915));
#16319=CARTESIAN_POINT('Ctrl Pts',(-6.13478909423228,2.86304904084892,11.2173381176655));
#16320=CARTESIAN_POINT('Ctrl Pts',(-5.51202996456676,2.96902046658306,11.3014313460436));
#16321=CARTESIAN_POINT('Ctrl Pts',(-5.04310782052529,3.38875866553956,11.3851878225675));
#16322=CARTESIAN_POINT('Ctrl Pts',(-4.92780437314741,3.78964966219835,11.4407823887586));
#16323=CARTESIAN_POINT('Ctrl Pts',(-4.9277773302074,3.99053173009658,11.468514508194));
#16324=CARTESIAN_POINT('Ctrl Pts',(-5.02992177076988,4.01367144562228,2.60093950625076));
#16325=CARTESIAN_POINT('Ctrl Pts',(-5.02994631566222,4.19599723747468,2.62610989942287));
#16326=CARTESIAN_POINT('Ctrl Pts',(-5.13442851066836,4.55976071314582,2.67654110121348));
#16327=CARTESIAN_POINT('Ctrl Pts',(-5.56134974573439,4.94238891673102,2.75283713624014));
#16328=CARTESIAN_POINT('Ctrl Pts',(-6.13078482073242,5.03959236213032,2.82972340704282));
#16329=CARTESIAN_POINT('Ctrl Pts',(-6.66903413561347,4.81735056602101,2.90723061263203));
#16330=CARTESIAN_POINT('Ctrl Pts',(-7.00920598700227,4.33896215278912,2.98534759690749));
#16331=CARTESIAN_POINT('Ctrl Pts',(-7.04301221179128,3.74836605021756,3.06407673097689));
#16332=CARTESIAN_POINT('Ctrl Pts',(-6.75522621874935,3.22631822149203,3.14340922597416));
#16333=CARTESIAN_POINT('Ctrl Pts',(-6.22990332689924,2.93525379627105,3.22333618102973));
#16334=CARTESIAN_POINT('Ctrl Pts',(-5.62589303937123,2.96854762030363,3.3038436934226));
#16335=CARTESIAN_POINT('Ctrl Pts',(-5.12873293812367,3.32056142076909,3.38491511731131));
#16336=CARTESIAN_POINT('Ctrl Pts',(-4.89352413204627,3.88691142159391,3.46653022944677));
#16337=CARTESIAN_POINT('Ctrl Pts',(-4.99635420577753,4.49544431396499,3.54866559717551));
#16338=CARTESIAN_POINT('Ctrl Pts',(-5.40970980407245,4.95874738227325,3.63129493312566));
#16339=CARTESIAN_POINT('Ctrl Pts',(-6.00949882097458,5.13204615047357,3.7143884170231));
#16340=CARTESIAN_POINT('Ctrl Pts',(-6.61281677753053,4.95875572754106,3.79791482865993));
#16341=CARTESIAN_POINT('Ctrl Pts',(-7.01751948399449,4.50615393741704,3.87872895502972));
#16342=CARTESIAN_POINT('Ctrl Pts',(-7.13278308470979,3.9361700979948,3.95675430685426));
#16343=CARTESIAN_POINT('Ctrl Pts',(-6.96798326611628,3.40093725384173,4.03191363881824));
#16344=CARTESIAN_POINT('Ctrl Pts',(-6.56588437170149,3.0085667161029,4.10730455915348));
#16345=CARTESIAN_POINT('Ctrl Pts',(-6.02380660015569,2.85552547105995,4.1828984645294));
#16346=CARTESIAN_POINT('Ctrl Pts',(-5.47331145361356,2.98131883984841,4.25866237696137));
#16347=CARTESIAN_POINT('Ctrl Pts',(-5.08474990971239,3.32433292134206,4.32823136806072));
#16348=CARTESIAN_POINT('Ctrl Pts',(-4.89877468361185,3.75115510083092,4.39155785124952));
#16349=CARTESIAN_POINT('Ctrl Pts',(-4.88295322239428,4.17012206891284,4.44859648966953));
#16350=CARTESIAN_POINT('Ctrl Pts',(-5.02160607801429,4.56601850940387,4.50566779869827));
#16351=CARTESIAN_POINT('Ctrl Pts',(-5.32551155281313,4.91976278214796,4.56909881469144));
#16352=CARTESIAN_POINT('Ctrl Pts',(-5.79947738774271,5.13357696487596,4.63887974785071));
#16353=CARTESIAN_POINT('Ctrl Pts',(-6.36490413396263,5.09095180204026,4.71498361809831));
#16354=CARTESIAN_POINT('Ctrl Pts',(-6.80123703014098,4.8090092395521,4.78468286989168));
#16355=CARTESIAN_POINT('Ctrl Pts',(-7.04805256548717,4.41489660565433,4.84798445867037));
#16356=CARTESIAN_POINT('Ctrl Pts',(-7.15336810542833,3.86676874930573,4.92386067095593));
#16357=CARTESIAN_POINT('Ctrl Pts',(-6.88627890876445,3.18474879109202,5.01849467324825));
#16358=CARTESIAN_POINT('Ctrl Pts',(-6.09541647887762,2.8046825266247,5.13164475831956));
#16359=CARTESIAN_POINT('Ctrl Pts',(-5.26193150367434,3.06284131663416,5.24427210695287));
#16360=CARTESIAN_POINT('Ctrl Pts',(-4.82877192593564,3.81499627184568,5.35628586566125));
#16361=CARTESIAN_POINT('Ctrl Pts',(-5.02163444704993,4.65554191876049,5.46759432075168));
#16362=CARTESIAN_POINT('Ctrl Pts',(-5.73037873412853,5.13706979243288,5.57811802779472));
#16363=CARTESIAN_POINT('Ctrl Pts',(-6.38289817874058,5.03711333080618,5.66341089394338));
#16364=CARTESIAN_POINT('Ctrl Pts',(-6.73374240825734,4.76966130879657,5.72399486558992));
#16365=CARTESIAN_POINT('Ctrl Pts',(-6.95338553801738,4.49503228262409,5.77232227188337));
#16366=CARTESIAN_POINT('Ctrl Pts',(-7.08535371842541,4.06660437649563,5.8324656844589));
#16367=CARTESIAN_POINT('Ctrl Pts',(-6.9787800468111,3.54300210723951,5.90419387832559));
#16368=CARTESIAN_POINT('Ctrl Pts',(-6.63720229094171,3.13634372816596,5.97547164377769));
#16369=CARTESIAN_POINT('Ctrl Pts',(-6.14599330113866,2.94418081803825,6.04628105868442));
#16370=CARTESIAN_POINT('Ctrl Pts',(-5.66932576801709,3.00445079184052,6.11075987344921));
#16371=CARTESIAN_POINT('Ctrl Pts',(-5.30755364968692,3.23270103855633,6.16902649445036));
#16372=CARTESIAN_POINT('Ctrl Pts',(-5.00263765117448,3.6439734402584,6.23858286226327));
#16373=CARTESIAN_POINT('Ctrl Pts',(-4.96258684153503,4.17541554580903,6.30760221503178));
#16374=CARTESIAN_POINT('Ctrl Pts',(-5.20013468158334,4.62018958382737,6.37607271900513));
#16375=CARTESIAN_POINT('Ctrl Pts',(-5.48418644663696,4.86495819379028,6.42715426330249));
#16376=CARTESIAN_POINT('Ctrl Pts',(-5.83700091859451,4.9879746399462,6.47796786909975));
#16377=CARTESIAN_POINT('Ctrl Pts',(-6.27014034257874,4.97194213569626,6.53693781695984));
#16378=CARTESIAN_POINT('Ctrl Pts',(-6.71018721911195,4.7285936197061,6.60390269044994));
#16379=CARTESIAN_POINT('Ctrl Pts',(-6.98138522201246,4.23654963479205,6.67865416688848));
#16380=CARTESIAN_POINT('Ctrl Pts',(-6.95464690173583,3.77319780008151,6.74048646026498));
#16381=CARTESIAN_POINT('Ctrl Pts',(-6.78949328491717,3.45466900883502,6.78967187976814));
#16382=CARTESIAN_POINT('Ctrl Pts',(-6.5850118543023,3.23821591657109,6.83051374195885));
#16383=CARTESIAN_POINT('Ctrl Pts',(-6.29417399113935,3.08462345483403,6.87525911245552));
#16384=CARTESIAN_POINT('Ctrl Pts',(-5.93944085316177,3.04484104332251,6.9238447927216));
#16385=CARTESIAN_POINT('Ctrl Pts',(-5.5386715025412,3.15204520558907,6.98028087779559));
#16386=CARTESIAN_POINT('Ctrl Pts',(-5.17945713800865,3.4731469683138,7.04445344266399));
#16387=CARTESIAN_POINT('Ctrl Pts',(-5.03071086209505,3.9913909494073,7.11621305131435));
#16388=CARTESIAN_POINT('Ctrl Pts',(-5.17946121358645,4.50630591590623,7.18758305156403));
#16389=CARTESIAN_POINT('Ctrl Pts',(-5.57742202874322,4.86150127118643,7.25859677523868));
#16390=CARTESIAN_POINT('Ctrl Pts',(-6.10098354551583,4.95012810222276,7.32929566337638));
#16391=CARTESIAN_POINT('Ctrl Pts',(-6.58957925866623,4.74746480607253,7.39972028560433));
#16392=CARTESIAN_POINT('Ctrl Pts',(-6.8944894280517,4.3173476510197,7.46991402598767));
#16393=CARTESIAN_POINT('Ctrl Pts',(-6.92380025037139,3.79233840638225,7.5399210681067));
#16394=CARTESIAN_POINT('Ctrl Pts',(-6.66985040219311,3.33310620512573,7.60978691749651));
#16395=CARTESIAN_POINT('Ctrl Pts',(-6.21114448179231,3.07967265445472,7.67955782005308));
#16396=CARTESIAN_POINT('Ctrl Pts',(-5.68826793231562,3.10905933047332,7.74928062518807));
#16397=CARTESIAN_POINT('Ctrl Pts',(-5.261141552189,3.41208503440244,7.81900242496648));
#16398=CARTESIAN_POINT('Ctrl Pts',(-5.06052819537421,3.89621323304842,7.88877035751342));
#16399=CARTESIAN_POINT('Ctrl Pts',(-5.14829035086678,4.41356981880071,7.95863124684226));
#16400=CARTESIAN_POINT('Ctrl Pts',(-5.49854581641565,4.80575214553667,8.02863150014836));
#16401=CARTESIAN_POINT('Ctrl Pts',(-6.00502473115743,4.95190610312972,8.09881641615639));
#16402=CARTESIAN_POINT('Ctrl Pts',(-6.51345932322945,4.80576316983501,8.16923087595341));
#16403=CARTESIAN_POINT('Ctrl Pts',(-6.85415432375228,4.4246714653667,8.23729907446955));
#16404=CARTESIAN_POINT('Ctrl Pts',(-6.95137144677235,3.94466951152941,8.30302428873296));
#16405=CARTESIAN_POINT('Ctrl Pts',(-6.81230057517098,3.49356736760953,8.3663911884946));
#16406=CARTESIAN_POINT('Ctrl Pts',(-6.50136287496873,3.18973077505633,8.42475462689054));
#16407=CARTESIAN_POINT('Ctrl Pts',(-6.13148243931581,3.06049314443402,8.47805277620172));
#16408=CARTESIAN_POINT('Ctrl Pts',(-5.77783212683701,3.07346287095625,8.52621486055624));
#16409=CARTESIAN_POINT('Ctrl Pts',(-5.45198580693692,3.21557058633095,8.57457908914575));
#16410=CARTESIAN_POINT('Ctrl Pts',(-5.19943688818408,3.46788583188274,8.62315687629181));
#16411=CARTESIAN_POINT('Ctrl Pts',(-5.05586062852743,3.7965510614861,8.67195580024494));
#16412=CARTESIAN_POINT('Ctrl Pts',(-5.04222328481417,4.15661669267005,8.72098352740896));
#16413=CARTESIAN_POINT('Ctrl Pts',(-5.16164350612221,4.49842329579526,8.77024741487185));
#16414=CARTESIAN_POINT('Ctrl Pts',(-5.39885118948844,4.77432531232921,8.8197540253094));
#16415=CARTESIAN_POINT('Ctrl Pts',(-5.72207722497841,4.94535456295086,8.86950941823545));
#16416=CARTESIAN_POINT('Ctrl Pts',(-6.08730982890222,4.98668115577665,8.91951882966172));
#16417=CARTESIAN_POINT('Ctrl Pts',(-6.44422838706502,4.89123320476848,8.96978715478432));
#16418=CARTESIAN_POINT('Ctrl Pts',(-6.74318709692094,4.67082128233194,9.02031790895771));
#16419=CARTESIAN_POINT('Ctrl Pts',(-6.94195573549741,4.35480362530798,9.0711154801606));
#16420=CARTESIAN_POINT('Ctrl Pts',(-7.01201283432467,3.98598307867038,9.12218006861651));
#16421=CARTESIAN_POINT('Ctrl Pts',(-6.94188012613974,3.61529685245114,9.17351903268827));
#16422=CARTESIAN_POINT('Ctrl Pts',(-6.71809166093455,3.25805588218288,9.23086040513767));
#16423=CARTESIAN_POINT('Ctrl Pts',(-6.32108019967002,3.00111879623715,9.2943252580824));
#16424=CARTESIAN_POINT('Ctrl Pts',(-5.80311451213473,2.96215959372275,9.36404554260668));
#16425=CARTESIAN_POINT('Ctrl Pts',(-5.30615754527745,3.18558411954849,9.4371657391009));
#16426=CARTESIAN_POINT('Ctrl Pts',(-4.97254369393785,3.65434309192426,9.51375567155646));
#16427=CARTESIAN_POINT('Ctrl Pts',(-4.93821839173336,4.25547436438888,9.59388220685397));
#16428=CARTESIAN_POINT('Ctrl Pts',(-5.23099161991045,4.78642955523378,9.67458401443596));
#16429=CARTESIAN_POINT('Ctrl Pts',(-5.76511389845588,5.0822907248545,9.75584348695941));
#16430=CARTESIAN_POINT('Ctrl Pts',(-6.37878715801708,5.04836955778898,9.83763916239741));
#16431=CARTESIAN_POINT('Ctrl Pts',(-6.88349050368107,4.69091453347305,9.91994670353367));
#16432=CARTESIAN_POINT('Ctrl Pts',(-7.12202289533655,4.11635206946976,10.0027386359648));
#16433=CARTESIAN_POINT('Ctrl Pts',(-7.01770835842206,3.49959201553773,10.0859846739843));
#16434=CARTESIAN_POINT('Ctrl Pts',(-6.59911145402226,3.03052923991246,10.1696518435186));
#16435=CARTESIAN_POINT('Ctrl Pts',(-5.99232502515886,2.85530579088301,10.2537046889382));
#16436=CARTESIAN_POINT('Ctrl Pts',(-5.38282080871405,3.03053423729314,10.3381054733215));
#16437=CARTESIAN_POINT('Ctrl Pts',(-4.95845861169447,3.50493632067857,10.4228143871725));
#16438=CARTESIAN_POINT('Ctrl Pts',(-4.85125090468359,4.13438025305609,10.5077898250386));
#16439=CARTESIAN_POINT('Ctrl Pts',(-5.09604965349032,4.72591478984614,10.5929885853316));
#16440=CARTESIAN_POINT('Ctrl Pts',(-5.61917028494442,5.09727783847887,10.6783661345901));
#16441=CARTESIAN_POINT('Ctrl Pts',(-6.26069397088939,5.13340762884881,10.7638768849291));
#16442=CARTESIAN_POINT('Ctrl Pts',(-6.82366484561828,4.82233127266765,10.8494744508988));
#16443=CARTESIAN_POINT('Ctrl Pts',(-7.1349559890951,4.25912401946948,10.9351119297844));
#16444=CARTESIAN_POINT('Ctrl Pts',(-7.09886085350935,3.61669627448514,11.0207420871626));
#16445=CARTESIAN_POINT('Ctrl Pts',(-6.726725604068,3.09227200005312,11.1063179076048));
#16446=CARTESIAN_POINT('Ctrl Pts',(-6.133342143185,2.84661696752136,11.1917922136962));
#16447=CARTESIAN_POINT('Ctrl Pts',(-5.5013537206857,2.95402140345727,11.2771193583949));
#16448=CARTESIAN_POINT('Ctrl Pts',(-5.02457058054561,3.3805972997307,11.3622524411556));
#16449=CARTESIAN_POINT('Ctrl Pts',(-4.90711056796205,3.78884348322686,11.4188571787799));
#16450=CARTESIAN_POINT('Ctrl Pts',(-4.90708301903907,3.99348412566317,11.4471081759781));
#16451=CARTESIAN_POINT('Ctrl Pts',(-5.08958602369426,4.0097422143856,2.62934334321296));
#16452=CARTESIAN_POINT('Ctrl Pts',(-5.08960909668988,4.18113437775253,2.65300432992655));
#16453=CARTESIAN_POINT('Ctrl Pts',(-5.18776711828874,4.52255313756382,2.70034320530108));
#16454=CARTESIAN_POINT('Ctrl Pts',(-5.58805341822381,4.8812003109688,2.77187303447584));
#16455=CARTESIAN_POINT('Ctrl Pts',(-6.12132268985396,4.97214168542557,2.84387592736578));
#16456=CARTESIAN_POINT('Ctrl Pts',(-6.6250405145593,4.76411472905679,2.9164168420007));
#16457=CARTESIAN_POINT('Ctrl Pts',(-6.94331845840803,4.31649001307946,2.98951192726223));
#16458=CARTESIAN_POINT('Ctrl Pts',(-6.9749746715728,3.76378663165257,3.0631944552253));
#16459=CARTESIAN_POINT('Ctrl Pts',(-6.70554141974671,3.27492468355936,3.13748515856724));
#16460=CARTESIAN_POINT('Ctrl Pts',(-6.21320712736269,3.00204398308599,3.21240526971059));
#16461=CARTESIAN_POINT('Ctrl Pts',(-5.64632516705992,3.03317798544545,3.28797050269457));
#16462=CARTESIAN_POINT('Ctrl Pts',(-5.17886703873242,3.36398699143602,3.36419356941742));
#16463=CARTESIAN_POINT('Ctrl Pts',(-4.95714819986703,3.89741137608331,3.44108294567733));
#16464=CARTESIAN_POINT('Ctrl Pts',(-5.05404278332218,4.47200014127016,3.51864333270601));
#16465=CARTESIAN_POINT('Ctrl Pts',(-5.44517543450279,4.91072858287447,3.59687538820991));
#16466=CARTESIAN_POINT('Ctrl Pts',(-6.01453304619026,5.07548882663536,3.67577584985644));
#16467=CARTESIAN_POINT('Ctrl Pts',(-6.58918617679193,4.91071236126573,3.75533744597375));
#16468=CARTESIAN_POINT('Ctrl Pts',(-6.97612300725113,4.4783911747965,3.83257829696492));
#16469=CARTESIAN_POINT('Ctrl Pts',(-7.08686193880412,3.93191614868384,3.90740355882087));
#16470=CARTESIAN_POINT('Ctrl Pts',(-6.92852875642478,3.4169390798757,3.97972468931771));
#16471=CARTESIAN_POINT('Ctrl Pts',(-6.54051538028299,3.03797533609853,4.05251872066026));
#16472=CARTESIAN_POINT('Ctrl Pts',(-6.01539730498932,2.88947896292994,4.1257687615144));
#16473=CARTESIAN_POINT('Ctrl Pts',(-5.48001097232824,3.01154598872243,4.19945421834644));
#16474=CARTESIAN_POINT('Ctrl Pts',(-5.10055444566604,3.34622164586703,4.2673806582065));
#16475=CARTESIAN_POINT('Ctrl Pts',(-4.91828161075229,3.76422683202926,4.32941580368313));
#16476=CARTESIAN_POINT('Ctrl Pts',(-4.90262739686774,4.17579135181212,4.38545682980996));
#16477=CARTESIAN_POINT('Ctrl Pts',(-5.0391283112046,4.56589122264886,4.44169556923536));
#16478=CARTESIAN_POINT('Ctrl Pts',(-5.33934590988134,4.9155506240904,4.50439033686248));
#16479=CARTESIAN_POINT('Ctrl Pts',(-5.80926478584637,5.12782619455085,4.57360252044762));
#16480=CARTESIAN_POINT('Ctrl Pts',(-6.37226870794527,5.0856772459095,4.64938417920319));
#16481=CARTESIAN_POINT('Ctrl Pts',(-6.80864308647832,4.80403298134512,4.71908085712304));
#16482=CARTESIAN_POINT('Ctrl Pts',(-7.05637578676585,4.40869807983537,4.78259624975845));
#16483=CARTESIAN_POINT('Ctrl Pts',(-7.16251945708551,3.85720809409794,4.85895651065945));
#16484=CARTESIAN_POINT('Ctrl Pts',(-6.89330101557501,3.16750144554567,4.95464513573224));
#16485=CARTESIAN_POINT('Ctrl Pts',(-6.08958867663454,2.78013704678207,5.06971861270507));
#16486=CARTESIAN_POINT('Ctrl Pts',(-5.23690622171536,3.04322519808429,5.1849241565956));
#16487=CARTESIAN_POINT('Ctrl Pts',(-4.7906499640607,3.81626968968653,5.3001367232004));
#16488=CARTESIAN_POINT('Ctrl Pts',(-4.9891869239238,4.68549381513598,5.41523683096681));
#16489=CARTESIAN_POINT('Ctrl Pts',(-5.72520324957272,5.18656740249823,5.53009936850738));
#16490=CARTESIAN_POINT('Ctrl Pts',(-6.40658390717164,5.08278139495824,5.61916700647108));
#16491=CARTESIAN_POINT('Ctrl Pts',(-6.77399210603382,4.80276068245273,5.6826055342916));
#16492=CARTESIAN_POINT('Ctrl Pts',(-7.00431863191779,4.51482589298084,5.73328075670049));
#16493=CARTESIAN_POINT('Ctrl Pts',(-7.14314022697556,4.06470659944838,5.79648179082563));
#16494=CARTESIAN_POINT('Ctrl Pts',(-7.03104691519316,3.51311217241579,5.87204065637758));
#16495=CARTESIAN_POINT('Ctrl Pts',(-6.67051256853736,3.08362473260782,5.94730439870082));
#16496=CARTESIAN_POINT('Ctrl Pts',(-6.15081617223352,2.88016159457978,6.02222877098954));
#16497=CARTESIAN_POINT('Ctrl Pts',(-5.64547668178805,2.94393293449389,6.09058436900044));
#16498=CARTESIAN_POINT('Ctrl Pts',(-5.26137505750651,3.1862109614243,6.15244231007988));
#16499=CARTESIAN_POINT('Ctrl Pts',(-4.93725546476308,3.62326890624268,6.22636752336837));
#16500=CARTESIAN_POINT('Ctrl Pts',(-4.89445496952149,4.18887354325382,6.29982377924026));
#16501=CARTESIAN_POINT('Ctrl Pts',(-5.14750606659487,4.66275895844425,6.37276832116607));
#16502=CARTESIAN_POINT('Ctrl Pts',(-5.45026508223206,4.92367181146985,6.4272143147893));
#16503=CARTESIAN_POINT('Ctrl Pts',(-5.82645426351564,5.05485739564245,6.4813918834484));
#16504=CARTESIAN_POINT('Ctrl Pts',(-6.28837776985666,5.03777053987273,6.54427717518941));
#16505=CARTESIAN_POINT('Ctrl Pts',(-6.75766182533428,4.77825976689007,6.6156816277228));
#16506=CARTESIAN_POINT('Ctrl Pts',(-7.04673661650366,4.25369878009071,6.69536196252822));
#16507=CARTESIAN_POINT('Ctrl Pts',(-7.01819649349061,3.76014401169988,6.76121469346688));
#16508=CARTESIAN_POINT('Ctrl Pts',(-6.842405554421,3.42113769275631,6.8135604237066));
#16509=CARTESIAN_POINT('Ctrl Pts',(-6.62491010422242,3.19092779055807,6.85699614151575));
#16510=CARTESIAN_POINT('Ctrl Pts',(-6.31584603200595,3.02775098386413,6.90453688382949));
#16511=CARTESIAN_POINT('Ctrl Pts',(-5.93934547183213,2.98556935104594,6.95609994689215));
#16512=CARTESIAN_POINT('Ctrl Pts',(-5.51459056401894,3.09925021805699,7.01590972758355));
#16513=CARTESIAN_POINT('Ctrl Pts',(-5.13474500286812,3.43902148798019,7.08377081623812));
#16514=CARTESIAN_POINT('Ctrl Pts',(-4.97805736011716,3.98577375141162,7.15945438099295));
#16515=CARTESIAN_POINT('Ctrl Pts',(-5.13473533545388,4.52718957327834,7.23449048550936));
#16516=CARTESIAN_POINT('Ctrl Pts',(-5.55197906444832,4.89921218790737,7.3088943913826));
#16517=CARTESIAN_POINT('Ctrl Pts',(-6.09862301928659,4.99143129445875,7.38268564523815));
#16518=CARTESIAN_POINT('Ctrl Pts',(-6.606479508496,4.78042080069058,7.4558871749407));
#16519=CARTESIAN_POINT('Ctrl Pts',(-6.92180017614838,4.33501283570147,7.52852551129164));
#16520=CARTESIAN_POINT('Ctrl Pts',(-6.95163025782033,3.79411735553687,7.6006304638527));
#16521=CARTESIAN_POINT('Ctrl Pts',(-6.69096189914452,3.32352522627327,7.67223500680259));
#16522=CARTESIAN_POINT('Ctrl Pts',(-6.22294780648661,3.06539982241649,7.74337508280607));
#16523=CARTESIAN_POINT('Ctrl Pts',(-5.69252682775021,3.09561549920305,7.81408937374553));
#16524=CARTESIAN_POINT('Ctrl Pts',(-5.26180726836289,3.40169439692029,7.88441907963459));
#16525=CARTESIAN_POINT('Ctrl Pts',(-5.06089205454407,3.88763262522401,7.9544076442884));
#16526=CARTESIAN_POINT('Ctrl Pts',(-5.14887297659026,4.40380377780348,8.02410059938868));
#16527=CARTESIAN_POINT('Ctrl Pts',(-5.49673854688707,4.79269430477356,8.09354506403565));
#16528=CARTESIAN_POINT('Ctrl Pts',(-5.9966646045048,4.93653868914869,8.16278992414471));
#16529=CARTESIAN_POINT('Ctrl Pts',(-6.49558078845043,4.79271917633619,8.23188451023252));
#16530=CARTESIAN_POINT('Ctrl Pts',(-6.8279254569334,4.42041712558591,8.29832525414164));
#16531=CARTESIAN_POINT('Ctrl Pts',(-6.92211402946376,3.954003052392,8.3621675915439));
#16532=CARTESIAN_POINT('Ctrl Pts',(-6.78734277050336,3.51770084265875,8.42345982961206));
#16533=CARTESIAN_POINT('Ctrl Pts',(-6.48766560070395,3.225159116655,8.4796752721566));
#16534=CARTESIAN_POINT('Ctrl Pts',(-6.1325704869422,3.10120573789478,8.53083075438161));
#16535=CARTESIAN_POINT('Ctrl Pts',(-5.79405420803016,3.11370858336792,8.57692520937968));
#16536=CARTESIAN_POINT('Ctrl Pts',(-5.4830197479851,3.24945336104646,8.62309331209753));
#16537=CARTESIAN_POINT('Ctrl Pts',(-5.24260300270298,3.48976277901665,8.66934329744669));
#16538=CARTESIAN_POINT('Ctrl Pts',(-5.10629115290446,3.80199725893422,8.71569288439519));
#16539=CARTESIAN_POINT('Ctrl Pts',(-5.09344018251244,4.14326532445679,8.76215618077292));
#16540=CARTESIAN_POINT('Ctrl Pts',(-5.20645717818496,4.4665333970135,8.80874723494016));
#16541=CARTESIAN_POINT('Ctrl Pts',(-5.43043962688319,4.72695400089958,8.8554796753622));
#16542=CARTESIAN_POINT('Ctrl Pts',(-5.73508248391682,4.88808365887862,8.90236685255007));
#16543=CARTESIAN_POINT('Ctrl Pts',(-6.0787635295149,4.92691816768683,8.9494215505399));
#16544=CARTESIAN_POINT('Ctrl Pts',(-6.41414963576881,4.83717952868894,8.99665644006685));
#16545=CARTESIAN_POINT('Ctrl Pts',(-6.69473020190159,4.6302656773445,9.04408299555505));
#16546=CARTESIAN_POINT('Ctrl Pts',(-6.88108457282113,4.3339202142424,9.09171380309133));
#16547=CARTESIAN_POINT('Ctrl Pts',(-6.94669400638978,3.98835022131002,9.13955729138141));
#16548=CARTESIAN_POINT('Ctrl Pts',(-6.88100497165465,3.64125145641925,9.1876294691536));
#16549=CARTESIAN_POINT('Ctrl Pts',(-6.6715256852485,3.30689107957766,9.24130014970914));
#16550=CARTESIAN_POINT('Ctrl Pts',(-6.3000268370675,3.06648207926289,9.30068636874497));
#16551=CARTESIAN_POINT('Ctrl Pts',(-5.81535571189857,3.03002056087319,9.36592627913045));
#16552=CARTESIAN_POINT('Ctrl Pts',(-5.35018368207742,3.23913151569331,9.43437243532255));
#16553=CARTESIAN_POINT('Ctrl Pts',(-5.03765642187869,3.67816124377273,9.50611601908226));
#16554=CARTESIAN_POINT('Ctrl Pts',(-5.0053771670949,4.2418152892366,9.58125441399916));
#16555=CARTESIAN_POINT('Ctrl Pts',(-5.28018936987031,4.74045258275521,9.65704272269345));
#16556=CARTESIAN_POINT('Ctrl Pts',(-5.78256486548921,5.01890213015692,9.73349228098031));
#16557=CARTESIAN_POINT('Ctrl Pts',(-6.36108012953608,4.98710397324951,9.81061023053686));
#16558=CARTESIAN_POINT('Ctrl Pts',(-6.8381331976359,4.6494838262545,9.88839989633978));
#16559=CARTESIAN_POINT('Ctrl Pts',(-7.06436608081689,4.10514848060083,9.96686058454078));
#16560=CARTESIAN_POINT('Ctrl Pts',(-6.96547905293281,3.51895521040063,10.0459876562616));
#16561=CARTESIAN_POINT('Ctrl Pts',(-6.56657813231277,3.07154766463719,10.1257725281815));
#16562=CARTESIAN_POINT('Ctrl Pts',(-5.98612686164896,2.90361920268451,10.2062027310299));
#16563=CARTESIAN_POINT('Ctrl Pts',(-5.40077082545841,3.07157466204263,10.2872619783505));
#16564=CARTESIAN_POINT('Ctrl Pts',(-4.99146624135684,3.52863915494167,10.3689302600859));
#16565=CARTESIAN_POINT('Ctrl Pts',(-4.88736373815124,4.1377465623043,10.451183968312));
#16566=CARTESIAN_POINT('Ctrl Pts',(-5.12491722559862,4.7127380657226,10.533996050922));
#16567=CARTESIAN_POINT('Ctrl Pts',(-5.63522883559405,5.07547609755517,10.6173360926148));
#16568=CARTESIAN_POINT('Ctrl Pts',(-6.26402278835794,5.11128141209404,10.7011706911434));
#16569=CARTESIAN_POINT('Ctrl Pts',(-6.81848369757312,4.80536147832042,10.7854632420856));
#16570=CARTESIAN_POINT('Ctrl Pts',(-7.12669178520415,4.24855993845081,10.8701750756115));
#16571=CARTESIAN_POINT('Ctrl Pts',(-7.09123147569517,3.61030668173643,10.9552635816668));
#16572=CARTESIAN_POINT('Ctrl Pts',(-6.72016314892057,3.08670479875095,11.0406872412903));
#16573=CARTESIAN_POINT('Ctrl Pts',(-6.12541064922602,2.84004009606229,11.1263951850926));
#16574=CARTESIAN_POINT('Ctrl Pts',(-5.48884100247513,2.94783409228307,11.2123513814334));
#16575=CARTESIAN_POINT('Ctrl Pts',(-5.00621523782245,3.37901620738018,11.2984814193147));
#16576=CARTESIAN_POINT('Ctrl Pts',(-4.88655208754281,3.79388081444679,11.3560322966674));
#16577=CARTESIAN_POINT('Ctrl Pts',(-4.8865240586904,4.00208649884007,11.3847754541186));
#16578=CARTESIAN_POINT('Ctrl Pts',(-5.11146420993595,3.99650690804392,2.72519407923183));
#16579=CARTESIAN_POINT('Ctrl Pts',(-5.11148671135746,4.16365327148895,2.74826892587012));
#16580=CARTESIAN_POINT('Ctrl Pts',(-5.2073387334252,4.4956152654922,2.79432434811692));
#16581=CARTESIAN_POINT('Ctrl Pts',(-5.59391925930553,4.84117169410349,2.86333869253526));
#16582=CARTESIAN_POINT('Ctrl Pts',(-6.10462940586839,4.92774917966529,2.93229835234812));
#16583=CARTESIAN_POINT('Ctrl Pts',(-6.58327176583413,4.7295348578091,3.00126579937436));
#16584=CARTESIAN_POINT('Ctrl Pts',(-6.88337501314833,4.30667247023342,3.07028767211521));
#16585=CARTESIAN_POINT('Ctrl Pts',(-6.91263235581757,3.78818989461597,3.13941738013105));
#16586=CARTESIAN_POINT('Ctrl Pts',(-6.66103458152486,3.33253551407342,3.2087045265732));
#16587=CARTESIAN_POINT('Ctrl Pts',(-6.20424810480219,3.07978627953998,3.27819919985182));
#16588=CARTESIAN_POINT('Ctrl Pts',(-5.68108649297066,3.10885755482802,3.3479496519015));
#16589=CARTESIAN_POINT('Ctrl Pts',(-5.25169620629678,3.41309053471004,3.41800286743285));
#16590=CARTESIAN_POINT('Ctrl Pts',(-5.04894523297885,3.90154084565558,3.48840393446534));
#16591=CARTESIAN_POINT('Ctrl Pts',(-5.13758046630622,4.42589822713349,3.5591959606558));
#16592=CARTESIAN_POINT('Ctrl Pts',(-5.49376253990945,4.82517927832118,3.63041966550646));
#16593=CARTESIAN_POINT('Ctrl Pts',(-6.01110718354508,4.97476701081733,3.70211331753018));
#16594=CARTESIAN_POINT('Ctrl Pts',(-6.53252812358959,4.82518146836992,3.77431221742951));
#16595=CARTESIAN_POINT('Ctrl Pts',(-6.88337346417075,4.43315294513001,3.84435516038971));
#16596=CARTESIAN_POINT('Ctrl Pts',(-6.98379294743255,3.93768269483383,3.91219940932669));
#16597=CARTESIAN_POINT('Ctrl Pts',(-6.84022481108866,3.47058194620396,3.97779629128527));
#16598=CARTESIAN_POINT('Ctrl Pts',(-6.4880568325447,3.12652942453571,4.04387572836497));
#16599=CARTESIAN_POINT('Ctrl Pts',(-6.0108137656867,2.99147239305588,4.11045064738684));
#16600=CARTESIAN_POINT('Ctrl Pts',(-5.5233657853622,3.10248135006783,4.1775341626934));
#16601=CARTESIAN_POINT('Ctrl Pts',(-5.17709342585232,3.40770238602073,4.23950070121029));
#16602=CARTESIAN_POINT('Ctrl Pts',(-5.01036803456119,3.78984364106918,4.29621638746104));
#16603=CARTESIAN_POINT('Ctrl Pts',(-4.99594479901417,4.1668986052098,4.34755687317996));
#16604=CARTESIAN_POINT('Ctrl Pts',(-5.12120361012274,4.52513375382838,4.39919526106358));
#16605=CARTESIAN_POINT('Ctrl Pts',(-5.39746462943087,4.84705650909992,4.45690227955026));
#16606=CARTESIAN_POINT('Ctrl Pts',(-5.83126731307521,5.04326241388392,4.52080469595619));
#16607=CARTESIAN_POINT('Ctrl Pts',(-6.35313532996607,5.00445569370675,4.59104399722636));
#16608=CARTESIAN_POINT('Ctrl Pts',(-6.75942140048203,4.74254821004542,4.65590506236411));
#16609=CARTESIAN_POINT('Ctrl Pts',(-6.99100458315705,4.37323249129891,4.71524509037977));
#16610=CARTESIAN_POINT('Ctrl Pts',(-7.09069411396853,3.85626121037699,4.78683233689444));
#16611=CARTESIAN_POINT('Ctrl Pts',(-6.83782768759017,3.20584888634675,4.87700820439253));
#16612=CARTESIAN_POINT('Ctrl Pts',(-6.07502780938017,2.83677943548265,4.98629119772695));
#16613=CARTESIAN_POINT('Ctrl Pts',(-5.25818762639893,3.08741236761678,5.09658082375559));
#16614=CARTESIAN_POINT('Ctrl Pts',(-4.82609468064246,3.83314196449917,5.20780897949353));
#16615=CARTESIAN_POINT('Ctrl Pts',(-5.01804196964182,4.68005730215182,5.31989208061913));
#16616=CARTESIAN_POINT('Ctrl Pts',(-5.74046220552027,5.17368997930613,5.43274493776054));
#16617=CARTESIAN_POINT('Ctrl Pts',(-6.41624680437255,5.07190602588026,5.52103403340694));
#16618=CARTESIAN_POINT('Ctrl Pts',(-6.78287311853616,4.79260968907092,5.58431543465606));
#16619=CARTESIAN_POINT('Ctrl Pts',(-7.01337901553013,4.50455289260236,5.63501963999642));
#16620=CARTESIAN_POINT('Ctrl Pts',(-7.15327228278993,4.05225837452208,5.69852711648277));
#16621=CARTESIAN_POINT('Ctrl Pts',(-7.04032973210259,3.49436664439344,5.7749325845684));
#16622=CARTESIAN_POINT('Ctrl Pts',(-6.67391452160444,3.05719409604593,5.85147827278331));
#16623=CARTESIAN_POINT('Ctrl Pts',(-6.14222098191702,2.84858797925773,5.92814825015341));
#16624=CARTESIAN_POINT('Ctrl Pts',(-5.62200447541444,2.9138522941561,5.99849597217976));
#16625=CARTESIAN_POINT('Ctrl Pts',(-5.2245261536068,3.16436876909183,6.06248327165541));
#16626=CARTESIAN_POINT('Ctrl Pts',(-4.88759619272133,3.61827656038866,6.13928274630519));
#16627=CARTESIAN_POINT('Ctrl Pts',(-4.84202233602887,4.20949050233905,6.21606350960167));
#16628=CARTESIAN_POINT('Ctrl Pts',(-5.10798876828044,4.70809462301289,6.29277587691175));
#16629=CARTESIAN_POINT('Ctrl Pts',(-5.42758183608149,4.9836863495513,6.35025953668304));
#16630=CARTESIAN_POINT('Ctrl Pts',(-5.82626078871504,5.12287862051017,6.40767598187554));
#16631=CARTESIAN_POINT('Ctrl Pts',(-6.31765994699635,5.10487041721485,6.47456839078133));
#16632=CARTESIAN_POINT('Ctrl Pts',(-6.81927831104067,4.8279461579424,6.55085139917529));
#16633=CARTESIAN_POINT('Ctrl Pts',(-7.13010460728862,4.26483633665069,6.63640932811157));
#16634=CARTESIAN_POINT('Ctrl Pts',(-7.09962536285686,3.73231937891717,6.70744540954714));
#16635=CARTESIAN_POINT('Ctrl Pts',(-6.90939545722011,3.36533955944663,6.76410161696636));
#16636=CARTESIAN_POINT('Ctrl Pts',(-6.67353014454027,3.11562305636599,6.81121005168782));
#16637=CARTESIAN_POINT('Ctrl Pts',(-6.33759434231894,2.93816086346153,6.86288612599481));
#16638=CARTESIAN_POINT('Ctrl Pts',(-5.9273264322903,2.89211004532868,6.91907330779778));
#16639=CARTESIAN_POINT('Ctrl Pts',(-5.46342269576929,3.01616830676018,6.98439039606857));
#16640=CARTESIAN_POINT('Ctrl Pts',(-5.04741643663609,3.38800643932693,7.05868193967993));
#16641=CARTESIAN_POINT('Ctrl Pts',(-4.87524080338402,3.98808878625817,7.1417508284993));
#16642=CARTESIAN_POINT('Ctrl Pts',(-5.04742888902791,4.58361105136446,7.22427616836105));
#16643=CARTESIAN_POINT('Ctrl Pts',(-5.50696177813016,4.99347012310367,7.30623032326481));
#16644=CARTESIAN_POINT('Ctrl Pts',(-6.10965855662746,5.09519407175069,7.38758749089929));
#16645=CARTESIAN_POINT('Ctrl Pts',(-6.66980784530153,4.86245512149429,7.46832609908296));
#16646=CARTESIAN_POINT('Ctrl Pts',(-7.01748273583442,4.37125721649622,7.54842792966416));
#16647=CARTESIAN_POINT('Ctrl Pts',(-7.05025029721227,3.77526621056693,7.6278786796359));
#16648=CARTESIAN_POINT('Ctrl Pts',(-6.76330668666928,3.25754943443463,7.70666784425883));
#16649=CARTESIAN_POINT('Ctrl Pts',(-6.24929824544846,2.97428480937579,7.78478885750138));
#16650=CARTESIAN_POINT('Ctrl Pts',(-5.66840638807499,3.00762386986153,7.86223910969369));
#16651=CARTESIAN_POINT('Ctrl Pts',(-5.19838941912511,3.34199008402616,7.93901995371726));
#16652=CARTESIAN_POINT('Ctrl Pts',(-4.98021840676051,3.87055262696194,8.0151367421138));
#16653=CARTESIAN_POINT('Ctrl Pts',(-5.0758490831127,4.42932105247054,8.09059869048116));
#16654=CARTESIAN_POINT('Ctrl Pts',(-5.45090874168749,4.84797551191977,8.16541907094984));
#16655=CARTESIAN_POINT('Ctrl Pts',(-5.98662713437262,5.00163881878175,8.23961458119776));
#16656=CARTESIAN_POINT('Ctrl Pts',(-6.51778625442196,4.84800086352156,8.31320648177161));
#16657=CARTESIAN_POINT('Ctrl Pts',(-6.86903664765677,4.4537703574742,8.38351367301843));
#16658=CARTESIAN_POINT('Ctrl Pts',(-6.96763730784423,3.96342515041434,8.45063523465213));
#16659=CARTESIAN_POINT('Ctrl Pts',(-6.82651993949993,3.50789653737747,8.5146520381989));
#16660=CARTESIAN_POINT('Ctrl Pts',(-6.51537470064459,3.20468645809038,8.57297673861431));
#16661=CARTESIAN_POINT('Ctrl Pts',(-6.14917583830804,3.07706708341011,8.62573355281478));
#16662=CARTESIAN_POINT('Ctrl Pts',(-5.80197126391332,3.09006782431164,8.6730209151348));
#16663=CARTESIAN_POINT('Ctrl Pts',(-5.48475623204359,3.22870238611783,8.7201215891855));
#16664=CARTESIAN_POINT('Ctrl Pts',(-5.24095954943397,3.47264590303982,8.76705526211315));
#16665=CARTESIAN_POINT('Ctrl Pts',(-5.10358476082081,3.78776518994619,8.81383109437915));
#16666=CARTESIAN_POINT('Ctrl Pts',(-5.09086869503226,4.13021000186943,8.86046253898069));
#16667=CARTESIAN_POINT('Ctrl Pts',(-5.20381253416027,4.45272962356915,8.90696307606029));
#16668=CARTESIAN_POINT('Ctrl Pts',(-5.42621366433013,4.71104091973399,8.95334665880885));
#16669=CARTESIAN_POINT('Ctrl Pts',(-5.72694035497815,4.86990159293225,8.99962743071014));
#16670=CARTESIAN_POINT('Ctrl Pts',(-6.0642778017449,4.9078453605195,9.04582000979757));
#16671=CARTESIAN_POINT('Ctrl Pts',(-6.39163490242547,4.82007995371208,9.09193880682701));
#16672=CARTESIAN_POINT('Ctrl Pts',(-6.66398013382079,4.61903047711367,9.13799939651309));
#16673=CARTESIAN_POINT('Ctrl Pts',(-6.8438526556467,4.33269428655929,9.184015344281));
#16674=CARTESIAN_POINT('Ctrl Pts',(-6.90674694774413,4.00055605675756,9.23000516247249));
#16675=CARTESIAN_POINT('Ctrl Pts',(-6.84379030170675,3.6686848472656,9.27597658179215));
#16676=CARTESIAN_POINT('Ctrl Pts',(-6.64428368612177,3.35056368320241,9.32706296798443));
#16677=CARTESIAN_POINT('Ctrl Pts',(-6.29248775761018,3.12327735296885,9.38328153460815));
#16678=CARTESIAN_POINT('Ctrl Pts',(-5.83641934789406,3.08928669055234,9.44467550183694));
#16679=CARTESIAN_POINT('Ctrl Pts',(-5.40123529858635,3.28526385412951,9.50873870009347));
#16680=CARTESIAN_POINT('Ctrl Pts',(-5.11066538229929,3.6941010991266,9.57552439669237));
#16681=CARTESIAN_POINT('Ctrl Pts',(-5.08114040909863,4.21597232833541,9.64510193793716));
#16682=CARTESIAN_POINT('Ctrl Pts',(-5.33465538188479,4.6753099831835,9.71495139697783));
#16683=CARTESIAN_POINT('Ctrl Pts',(-5.79581996002734,4.93059943387018,9.78511888244445));
#16684=CARTESIAN_POINT('Ctrl Pts',(-6.32483627711044,4.90128596697204,9.8556490605078));
#16685=CARTESIAN_POINT('Ctrl Pts',(-6.75969561822109,4.59329231159124,9.92658419793803));
#16686=CARTESIAN_POINT('Ctrl Pts',(-6.96535793748658,4.09806931552254,9.99796426902674));
#16687=CARTESIAN_POINT('Ctrl Pts',(-6.87545751761248,3.56575269834969,10.0698265663819));
#16688=CARTESIAN_POINT('Ctrl Pts',(-6.51356552579593,3.15993629343994,10.14220553172));
#16689=CARTESIAN_POINT('Ctrl Pts',(-5.98728606474299,3.00768901099732,10.2151325409728));
#16690=CARTESIAN_POINT('Ctrl Pts',(-5.45650233408849,3.1599478008427,10.2886357289696));
#16691=CARTESIAN_POINT('Ctrl Pts',(-5.08505427049296,3.57461637569863,10.3627398332933));
#16692=CARTESIAN_POINT('Ctrl Pts',(-4.99035571726364,4.12795704288266,10.437466010666));
#16693=CARTESIAN_POINT('Ctrl Pts',(-5.20639519921345,4.65131594928899,10.512831779153));
#16694=CARTESIAN_POINT('Ctrl Pts',(-5.67176741775253,4.98236962341372,10.5888508190908));
#16695=CARTESIAN_POINT('Ctrl Pts',(-6.24692306139383,5.01537477896922,10.6655330858597));
#16696=CARTESIAN_POINT('Ctrl Pts',(-6.75589224783495,4.73489188265989,10.7428843299171));
#16697=CARTESIAN_POINT('Ctrl Pts',(-7.04007219825167,4.22219270063654,10.8209070256255));
#16698=CARTESIAN_POINT('Ctrl Pts',(-7.00764788063291,3.63187265532301,10.8995982295234));
#16699=CARTESIAN_POINT('Ctrl Pts',(-6.66325059419008,3.14520426747428,10.9789543736926));
#16700=CARTESIAN_POINT('Ctrl Pts',(-6.10819988711464,2.91453849274314,11.058960661495));
#16701=CARTESIAN_POINT('Ctrl Pts',(-5.51080240970513,3.01525157871369,11.1396149610308));
#16702=CARTESIAN_POINT('Ctrl Pts',(-5.0551220869379,3.42171950959631,11.2208744527486));
#16703=CARTESIAN_POINT('Ctrl Pts',(-4.94129981546046,3.8153290367668,11.2754818329556));
#16704=CARTESIAN_POINT('Ctrl Pts',(-4.94127315000938,4.01340701770439,11.302826843301));
#16705=CARTESIAN_POINT('Ctrl Pts',(-5.04970739996704,3.98586593555859,2.80233389724905));
#16706=CARTESIAN_POINT('Ctrl Pts',(-5.04973139993852,4.16414391474371,2.82694548283125));
#16707=CARTESIAN_POINT('Ctrl Pts',(-5.15207273229177,4.51778429231705,2.87600729424782));
#16708=CARTESIAN_POINT('Ctrl Pts',(-5.56143445144235,4.88296414226877,2.94901032448266));
#16709=CARTESIAN_POINT('Ctrl Pts',(-6.09813035455802,4.97345393073418,3.02146383671977));
#16710=CARTESIAN_POINT('Ctrl Pts',(-6.59717772837509,4.76616692282312,3.0933916160425));
#16711=CARTESIAN_POINT('Ctrl Pts',(-6.90734650210006,4.32810391152191,3.16483090871071));
#16712=CARTESIAN_POINT('Ctrl Pts',(-6.93678565771805,3.79557382692573,3.2358172810944));
#16713=CARTESIAN_POINT('Ctrl Pts',(-6.67992988144025,3.33168204106518,3.30639099867147));
#16714=CARTESIAN_POINT('Ctrl Pts',(-6.21810435684495,3.07685645369217,3.37659383904583));
#16715=CARTESIAN_POINT('Ctrl Pts',(-5.69393812253209,3.10660642536628,3.4464702010732));
#16716=CARTESIAN_POINT('Ctrl Pts',(-5.26762996911266,3.40941101795258,3.5160661735816));
#16717=CARTESIAN_POINT('Ctrl Pts',(-5.06839285544546,3.89098009041129,3.58542962758082));
#16718=CARTESIAN_POINT('Ctrl Pts',(-5.15561189334424,4.4033880452795,3.65460971073016));
#16719=CARTESIAN_POINT('Ctrl Pts',(-5.50139878752267,4.79014597346869,3.72365678087616));
#16720=CARTESIAN_POINT('Ctrl Pts',(-5.99929163750598,4.93352930590794,3.79262165568086));
#16721=CARTESIAN_POINT('Ctrl Pts',(-6.4970686585488,4.79016609531092,3.86155633018706));
#16722=CARTESIAN_POINT('Ctrl Pts',(-6.82936311892864,4.41814025925142,3.92795746104432));
#16723=CARTESIAN_POINT('Ctrl Pts',(-6.92363065152845,3.95125657284996,3.99187048957157));
#16724=CARTESIAN_POINT('Ctrl Pts',(-6.78882509008231,3.51372124013338,4.05331919673356));
#16725=CARTESIAN_POINT('Ctrl Pts',(-6.46039659394628,3.19327537628355,4.1148982207543));
#16726=CARTESIAN_POINT('Ctrl Pts',(-6.01766263256043,3.06825894175095,4.17664315434586));
#16727=CARTESIAN_POINT('Ctrl Pts',(-5.5675895656199,3.17101321438884,4.23858675780122));
#16728=CARTESIAN_POINT('Ctrl Pts',(-5.2492248404407,3.45189468829417,4.29557696959262));
#16729=CARTESIAN_POINT('Ctrl Pts',(-5.09642736304692,3.80234899603894,4.34758087720494));
#16730=CARTESIAN_POINT('Ctrl Pts',(-5.08330770876435,4.14729318609475,4.39454534850842));
#16731=CARTESIAN_POINT('Ctrl Pts',(-5.19772169901104,4.47431107671478,4.441684267873));
#16732=CARTESIAN_POINT('Ctrl Pts',(-5.44952133586914,4.76762287208321,4.49426708034093));
#16733=CARTESIAN_POINT('Ctrl Pts',(-5.84415803931418,4.94600136701132,4.5523911097729));
#16734=CARTESIAN_POINT('Ctrl Pts',(-6.31810385031458,4.91067419089945,4.61618003218375));
#16735=CARTESIAN_POINT('Ctrl Pts',(-6.68665036777128,4.67303306472473,4.67501868351521));
#16736=CARTESIAN_POINT('Ctrl Pts',(-6.89661632842578,4.33816644176502,4.72882134047227));
#16737=CARTESIAN_POINT('Ctrl Pts',(-6.98697202988125,3.86952263883875,4.79371605024056));
#16738=CARTESIAN_POINT('Ctrl Pts',(-6.75778190933801,3.27983692309617,4.87546960451597));
#16739=CARTESIAN_POINT('Ctrl Pts',(-6.06554426147497,2.94465225979484,4.97466219153242));
#16740=CARTESIAN_POINT('Ctrl Pts',(-5.32245651643167,3.17225925098387,5.07498410984188));
#16741=CARTESIAN_POINT('Ctrl Pts',(-4.92778951573427,3.85238246698133,5.17647141255265));
#16742=CARTESIAN_POINT('Ctrl Pts',(-5.10298048742041,4.62825658707493,5.2791449880962));
#16743=CARTESIAN_POINT('Ctrl Pts',(-5.76740082109715,5.08320984683702,5.38301457542082));
#16744=CARTESIAN_POINT('Ctrl Pts',(-6.39288814393051,4.98967356366879,5.46472968699651));
#16745=CARTESIAN_POINT('Ctrl Pts',(-6.73362172606756,4.73018672825182,5.5235334168208));
#16746=CARTESIAN_POINT('Ctrl Pts',(-6.94828598379921,4.46199079666324,5.57074911296363));
#16747=CARTESIAN_POINT('Ctrl Pts',(-7.07921409875927,4.03950241918021,5.63009246753764));
#16748=CARTESIAN_POINT('Ctrl Pts',(-6.9735205483604,3.5158079784997,5.70180655151957));
#16749=CARTESIAN_POINT('Ctrl Pts',(-6.62817002994743,3.10326385951304,5.77401639409909));
#16750=CARTESIAN_POINT('Ctrl Pts',(-6.12427120584258,2.90518634266498,5.84670069278975));
#16751=CARTESIAN_POINT('Ctrl Pts',(-5.62844987755089,2.96705262654286,5.9137529058833));
#16752=CARTESIAN_POINT('Ctrl Pts',(-5.24775397880409,3.20681158618404,5.97503027044029));
#16753=CARTESIAN_POINT('Ctrl Pts',(-4.92361176447729,3.64307030441914,6.04888078550589));
#16754=CARTESIAN_POINT('Ctrl Pts',(-4.8786775738425,4.21508342665461,6.12319606633034));
#16755=CARTESIAN_POINT('Ctrl Pts',(-5.13751318684674,4.70093420047505,6.19792703986058));
#16756=CARTESIAN_POINT('Ctrl Pts',(-5.45008477387499,4.97066958629773,6.25417272725587));
#16757=CARTESIAN_POINT('Ctrl Pts',(-5.84182005939013,5.10763090725229,6.31060530459667));
#16758=CARTESIAN_POINT('Ctrl Pts',(-6.32690143544471,5.09006208723829,6.37664516231843));
#16759=CARTESIAN_POINT('Ctrl Pts',(-6.82513596476563,4.81560943649251,6.45239369084021));
#16760=CARTESIAN_POINT('Ctrl Pts',(-7.13638106409612,4.25305528894405,6.53792591144884));
#16761=CARTESIAN_POINT('Ctrl Pts',(-7.10620757956584,3.71708032928425,6.60943336872173));
#16762=CARTESIAN_POINT('Ctrl Pts',(-6.91387605566801,3.34581492491729,6.66674540205016));
#16763=CARTESIAN_POINT('Ctrl Pts',(-6.67455235910194,3.09232127351564,6.71456126034345));
#16764=CARTESIAN_POINT('Ctrl Pts',(-6.33233370578708,2.91134781627226,6.76722279147881));
#16765=CARTESIAN_POINT('Ctrl Pts',(-5.91245972381307,2.86404826449612,6.82473115868907));
#16766=CARTESIAN_POINT('Ctrl Pts',(-5.43553481296477,2.9913708635829,6.89188065995733));
#16767=CARTESIAN_POINT('Ctrl Pts',(-5.00519657260536,3.37532227919306,6.96868491584719));
#16768=CARTESIAN_POINT('Ctrl Pts',(-4.82552411217367,3.99939259114819,7.0551070900708));
#16769=CARTESIAN_POINT('Ctrl Pts',(-5.00521412307785,4.62290028123384,7.14150024752713));
#16770=CARTESIAN_POINT('Ctrl Pts',(-5.48875025669925,5.05490216838407,7.22781063449205));
#16771=CARTESIAN_POINT('Ctrl Pts',(-6.1269972684323,5.16315762594082,7.31398827930353));
#16772=CARTESIAN_POINT('Ctrl Pts',(-6.72373757857285,4.91575192086015,7.3999824846241));
#16773=CARTESIAN_POINT('Ctrl Pts',(-7.09632491756847,4.39016444565846,7.48574427967905));
#16774=CARTESIAN_POINT('Ctrl Pts',(-7.13200989794504,3.74901013706194,7.57122577023266));
#16775=CARTESIAN_POINT('Ctrl Pts',(-6.82225282779296,3.18930878099883,7.65638085980697));
#16776=CARTESIAN_POINT('Ctrl Pts',(-6.26460829902145,2.88158315511726,7.7411652953409));
#16777=CARTESIAN_POINT('Ctrl Pts',(-5.63181412213981,2.91757758974348,7.82553705211258));
#16778=CARTESIAN_POINT('Ctrl Pts',(-5.11795160772848,3.28278984563098,7.90945653702931));
#16779=CARTESIAN_POINT('Ctrl Pts',(-4.8786033228671,3.86203570830463,7.99288684593522));
#16780=CARTESIAN_POINT('Ctrl Pts',(-4.9834784860068,4.47596055036701,8.07579394079288));
#16781=CARTESIAN_POINT('Ctrl Pts',(-5.39619233550684,4.93686361644705,8.15814693095131));
#16782=CARTESIAN_POINT('Ctrl Pts',(-5.98659329122227,5.10631370816378,8.23991813342875));
#16783=CARTESIAN_POINT('Ctrl Pts',(-6.57245089294751,4.93690501920364,8.32108349554828));
#16784=CARTESIAN_POINT('Ctrl Pts',(-6.95992631722877,4.50201262961247,8.39863923032397));
#16785=CARTESIAN_POINT('Ctrl Pts',(-7.0686214319773,3.96129877129402,8.47264955664533));
#16786=CARTESIAN_POINT('Ctrl Pts',(-6.91307368893838,3.45942867756379,8.54318002431797));
#16787=CARTESIAN_POINT('Ctrl Pts',(-6.57065452508007,3.12585974988192,8.60735189964973));
#16788=CARTESIAN_POINT('Ctrl Pts',(-6.16834178931565,2.9857181819638,8.66530488614999));
#16789=CARTESIAN_POINT('Ctrl Pts',(-5.78753543501327,3.00003230773149,8.71716373843041));
#16790=CARTESIAN_POINT('Ctrl Pts',(-5.4403035260536,3.15186461292756,8.76872364368885));
#16791=CARTESIAN_POINT('Ctrl Pts',(-5.17405053055488,3.41838442867686,8.8199853550893));
#16792=CARTESIAN_POINT('Ctrl Pts',(-5.02443569797404,3.76179608763484,8.87095033478593));
#16793=CARTESIAN_POINT('Ctrl Pts',(-5.01071112624326,4.13394596082485,8.92162060989388));
#16794=CARTESIAN_POINT('Ctrl Pts',(-5.13318588183195,4.48337012347238,8.97199917604928));
#16795=CARTESIAN_POINT('Ctrl Pts',(-5.37347503109835,4.76228741366554,9.02208969182068));
#16796=CARTESIAN_POINT('Ctrl Pts',(-5.69721116839696,4.93316838834119,9.07189665925581));
#16797=CARTESIAN_POINT('Ctrl Pts',(-6.0589731200314,4.9737322857,9.1214252117248));
#16798=CARTESIAN_POINT('Ctrl Pts',(-6.40861121955068,4.8798544518055,9.1706814415999));
#16799=CARTESIAN_POINT('Ctrl Pts',(-6.69823740111901,4.6658728811842,9.2196716693642));
#16800=CARTESIAN_POINT('Ctrl Pts',(-6.88862583552788,4.36251796004086,9.26840400845727));
#16801=CARTESIAN_POINT('Ctrl Pts',(-6.95478616822326,4.01229514034741,9.31688480847724));
#16802=CARTESIAN_POINT('Ctrl Pts',(-6.88856176972145,3.66404742277028,9.36512658585856));
#16803=CARTESIAN_POINT('Ctrl Pts',(-6.68005169721061,3.33191633214502,9.41846778625709));
#16804=CARTESIAN_POINT('Ctrl Pts',(-6.31460669315386,3.09625457845185,9.47682666960199));
#16805=CARTESIAN_POINT('Ctrl Pts',(-5.84434359292178,3.06162099030016,9.54012231568025));
#16806=CARTESIAN_POINT('Ctrl Pts',(-5.39899847593867,3.26265748297777,9.60569442922599));
#16807=CARTESIAN_POINT('Ctrl Pts',(-5.10429076867847,3.67833278879711,9.67352609353735));
#16808=CARTESIAN_POINT('Ctrl Pts',(-5.07516908125756,4.20415060051834,9.74361156651549));
#16809=CARTESIAN_POINT('Ctrl Pts',(-5.3290043949544,4.66278566701131,9.81338623218308));
#16810=CARTESIAN_POINT('Ctrl Pts',(-5.78623808748219,4.91519435249182,9.88289701703703));
#16811=CARTESIAN_POINT('Ctrl Pts',(-6.3060517965798,4.88578370031614,9.95219212118266));
#16812=CARTESIAN_POINT('Ctrl Pts',(-6.72957149563769,4.58509644581646,10.0213211404762));
#16813=CARTESIAN_POINT('Ctrl Pts',(-6.92791848165719,4.10599187307524,10.0903346248714));
#16814=CARTESIAN_POINT('Ctrl Pts',(-6.84110398927473,3.5952641796134,10.1592838512015));
#16815=CARTESIAN_POINT('Ctrl Pts',(-6.49597787726478,3.2090411855636,10.2282204510126));
#16816=CARTESIAN_POINT('Ctrl Pts',(-5.99800352137511,3.06550216277556,10.2971961468308));
#16817=CARTESIAN_POINT('Ctrl Pts',(-5.49932225007621,3.20903924367168,10.3662624291035));
#16818=CARTESIAN_POINT('Ctrl Pts',(-5.15269705665512,3.59664731894394,10.4354702785398));
#16819=CARTESIAN_POINT('Ctrl Pts',(-5.06513063256634,4.11067041794936,10.5048698000626));
#16820=CARTESIAN_POINT('Ctrl Pts',(-5.26510991061431,4.59418295823839,10.5745100007069));
#16821=CARTESIAN_POINT('Ctrl Pts',(-5.69342119822868,4.89848196985741,10.6444384472408));
#16822=CARTESIAN_POINT('Ctrl Pts',(-6.22048565505005,4.92845041025329,10.7147010475278));
#16823=CARTESIAN_POINT('Ctrl Pts',(-6.68521940982778,4.67207850548342,10.7853416191958));
#16824=CARTESIAN_POINT('Ctrl Pts',(-6.9438915773895,4.20500647688942,10.8564020052726));
#16825=CARTESIAN_POINT('Ctrl Pts',(-6.91427609532709,3.66847163030632,10.9279210525427));
#16826=CARTESIAN_POINT('Ctrl Pts',(-6.60163877912294,3.22685146759834,10.9999360420128));
#16827=CARTESIAN_POINT('Ctrl Pts',(-6.0983327490694,3.01775518242327,11.0724787983336));
#16828=CARTESIAN_POINT('Ctrl Pts',(-5.55680569487759,3.10903241001865,11.1455837409093));
#16829=CARTESIAN_POINT('Ctrl Pts',(-5.14359296425941,3.47760759058162,11.2192690442149));
#16830=CARTESIAN_POINT('Ctrl Pts',(-5.04025170604376,3.83468368477443,11.2688070752426));
#16831=CARTESIAN_POINT('Ctrl Pts',(-5.04022747391784,4.01468628666098,11.2936567480204));
#16832=CARTESIAN_POINT('Ctrl Pts',(-4.95040447126516,3.98592256360826,2.80202053804765));
#16833=CARTESIAN_POINT('Ctrl Pts',(-4.95043091003926,4.18231659775015,2.82913307657434));
#16834=CARTESIAN_POINT('Ctrl Pts',(-5.06329226241015,4.57248759339974,2.88326752141538));
#16835=CARTESIAN_POINT('Ctrl Pts',(-5.51486202834107,4.97524472192967,2.96379225597859));
#16836=CARTESIAN_POINT('Ctrl Pts',(-6.10665528742512,5.07498487533097,3.04369205371294));
#16837=CARTESIAN_POINT('Ctrl Pts',(-6.65633239830572,4.84652999270038,3.12292773711241));
#16838=CARTESIAN_POINT('Ctrl Pts',(-6.9973108765322,4.36466637062073,3.20150215875154));
#16839=CARTESIAN_POINT('Ctrl Pts',(-7.02939784011567,3.78028500733267,3.27940500864084));
#16840=CARTESIAN_POINT('Ctrl Pts',(-6.74810299878159,3.2728050208645,3.35663748365564));
#16841=CARTESIAN_POINT('Ctrl Pts',(-6.24433664339929,2.99519254130349,3.43320130422444));
#16842=CARTESIAN_POINT('Ctrl Pts',(-5.67505771277393,3.02785856483236,3.50910363511194));
#16843=CARTESIAN_POINT('Ctrl Pts',(-5.21440091341081,3.35554690775124,3.58435485999818));
#16844=CARTESIAN_POINT('Ctrl Pts',(-5.00051500372563,3.87366133572611,3.65896947953506));
#16845=CARTESIAN_POINT('Ctrl Pts',(-5.09425563285267,4.42157185945799,3.73296568547931));
#16846=CARTESIAN_POINT('Ctrl Pts',(-5.462150310971,4.83229878934543,3.80636524550889));
#16847=CARTESIAN_POINT('Ctrl Pts',(-5.98798150593187,4.98317282253211,3.87919373094752));
#16848=CARTESIAN_POINT('Ctrl Pts',(-6.50969648071242,4.83232792366873,3.95147945989542));
#16849=CARTESIAN_POINT('Ctrl Pts',(-6.85508457642829,4.44480762082077,4.02059709639111));
#16850=CARTESIAN_POINT('Ctrl Pts',(-6.95204190315741,3.96238793059401,4.08663859114721));
#16851=CARTESIAN_POINT('Ctrl Pts',(-6.81334677614592,3.5136697530612,4.14969044049817));
#16852=CARTESIAN_POINT('Ctrl Pts',(-6.47855613316745,3.18760750471201,4.21241950435217));
#16853=CARTESIAN_POINT('Ctrl Pts',(-6.03081518894969,3.06163527614584,4.27485530762707));
#16854=CARTESIAN_POINT('Ctrl Pts',(-5.57924400076306,3.16517210684398,4.33702916331017));
#16855=CARTESIAN_POINT('Ctrl Pts',(-5.26235852783461,3.44527804080697,4.39381651555624));
#16856=CARTESIAN_POINT('Ctrl Pts',(-5.11131528474039,3.79220578079815,4.44529570200474));
#16857=CARTESIAN_POINT('Ctrl Pts',(-5.09857586586284,4.13174734281154,4.4915318677947));
#16858=CARTESIAN_POINT('Ctrl Pts',(-5.21073898163706,4.45182214864689,4.53768640690343));
#16859=CARTESIAN_POINT('Ctrl Pts',(-5.45607191503352,4.73730787660388,4.5888965218401));
#16860=CARTESIAN_POINT('Ctrl Pts',(-5.83811149272645,4.90959852119948,4.64515384022942));
#16861=CARTESIAN_POINT('Ctrl Pts',(-6.2935786023769,4.87526943519902,4.70646656906679));
#16862=CARTESIAN_POINT('Ctrl Pts',(-6.64527957947667,4.64809167136525,4.76265837292092));
#16863=CARTESIAN_POINT('Ctrl Pts',(-6.84450663785382,4.3300747306855,4.81375039303616));
#16864=CARTESIAN_POINT('Ctrl Pts',(-6.92971145133925,3.88705234376868,4.87509302326313));
#16865=CARTESIAN_POINT('Ctrl Pts',(-6.71365998929187,3.33363363074556,4.95188314417723));
#16866=CARTESIAN_POINT('Ctrl Pts',(-6.06835226953183,3.02231338852184,5.04430471261663));
#16867=CARTESIAN_POINT('Ctrl Pts',(-5.38124050124584,3.23368703501002,5.13712614542432));
#16868=CARTESIAN_POINT('Ctrl Pts',(-5.0189980927801,3.85941422069564,5.23045662938603));
#16869=CARTESIAN_POINT('Ctrl Pts',(-5.17987791457587,4.56911666397937,5.32440725702233));
#16870=CARTESIAN_POINT('Ctrl Pts',(-5.78561808497084,4.98333190955499,5.41907560362953));
#16871=CARTESIAN_POINT('Ctrl Pts',(-6.35398858774582,4.89810415389661,5.49334391945794));
#16872=CARTESIAN_POINT('Ctrl Pts',(-6.66324728871676,4.66257986013562,5.54671917380987));
#16873=CARTESIAN_POINT('Ctrl Pts',(-6.85799457461404,4.41925435012529,5.58955592004314));
#16874=CARTESIAN_POINT('Ctrl Pts',(-6.97670080803186,4.03614191365389,5.64337065998053));
#16875=CARTESIAN_POINT('Ctrl Pts',(-6.88088708133519,3.56137269665567,5.7083859866602));
#16876=CARTESIAN_POINT('Ctrl Pts',(-6.56774877139036,3.18724959659898,5.7738673544995));
#16877=CARTESIAN_POINT('Ctrl Pts',(-6.1105137674248,3.00745058984831,5.83982431290547));
#16878=CARTESIAN_POINT('Ctrl Pts',(-5.6600605012146,3.06356690480529,5.90073862619864));
#16879=CARTESIAN_POINT('Ctrl Pts',(-5.31369872683335,3.28164279863364,5.95648275503902));
#16880=CARTESIAN_POINT('Ctrl Pts',(-5.01835072945631,3.67901092443548,6.02376014793761));
#16881=CARTESIAN_POINT('Ctrl Pts',(-4.97697944716172,4.20135318239159,6.09162170691514));
#16882=CARTESIAN_POINT('Ctrl Pts',(-5.21397626606511,4.64650539147114,6.16007680229855));
#16883=CARTESIAN_POINT('Ctrl Pts',(-5.5009097172886,4.89421993891025,6.21171562591074));
#16884=CARTESIAN_POINT('Ctrl Pts',(-5.86142976014365,5.02037373217275,6.2636524977601));
#16885=CARTESIAN_POINT('Ctrl Pts',(-6.30907789606985,5.0042822573264,6.32459304266943));
#16886=CARTESIAN_POINT('Ctrl Pts',(-6.77062818691674,4.75041637394186,6.39473198710031));
#16887=CARTESIAN_POINT('Ctrl Pts',(-7.06056473245011,4.22724802877586,6.47429953400173));
#16888=CARTESIAN_POINT('Ctrl Pts',(-7.03270980954092,3.72610700206045,6.5411448644184));
#16889=CARTESIAN_POINT('Ctrl Pts',(-6.85223257332155,3.37754933099021,6.59494075166314));
#16890=CARTESIAN_POINT('Ctrl Pts',(-6.62701654047639,3.13891117911654,6.63994397935717));
#16891=CARTESIAN_POINT('Ctrl Pts',(-6.30392790977769,2.96790294404537,6.68966570919111));
#16892=CARTESIAN_POINT('Ctrl Pts',(-5.90593173628063,2.92292306099434,6.74417633692474));
#16893=CARTESIAN_POINT('Ctrl Pts',(-5.45202916168621,3.04391154370486,6.80807460735696));
#16894=CARTESIAN_POINT('Ctrl Pts',(-5.04014333934976,3.41076195351744,6.88151530639827));
#16895=CARTESIAN_POINT('Ctrl Pts',(-4.86667543386624,4.01122016423334,6.96467649603348));
#16896=CARTESIAN_POINT('Ctrl Pts',(-5.04017668893253,4.61531134117894,7.0483417461296));
#16897=CARTESIAN_POINT('Ctrl Pts',(-5.51121666827128,5.03693972368687,7.13247718837409));
#16898=CARTESIAN_POINT('Ctrl Pts',(-6.1375489230342,5.14378348705712,7.21704382881911));
#16899=CARTESIAN_POINT('Ctrl Pts',(-6.72743578865273,4.8998792887582,7.30200118857734));
#16900=CARTESIAN_POINT('Ctrl Pts',(-7.09860950001123,4.37735225371753,7.38730600603053));
#16901=CARTESIAN_POINT('Ctrl Pts',(-7.13497166725086,3.73517172118145,7.47291318935821));
#16902=CARTESIAN_POINT('Ctrl Pts',(-6.82312529085993,3.17041778969823,7.55877577981912));
#16903=CARTESIAN_POINT('Ctrl Pts',(-6.25722282340157,2.85743337580234,7.64484533044293));
#16904=CARTESIAN_POINT('Ctrl Pts',(-5.61036515969932,2.89361956155909,7.73107215137484));
#16905=CARTESIAN_POINT('Ctrl Pts',(-5.08128094643061,3.26891729705054,7.81740565235628));
#16906=CARTESIAN_POINT('Ctrl Pts',(-4.83286127115891,3.86858697173099,7.90379456689586));
#16907=CARTESIAN_POINT('Ctrl Pts',(-4.94160324819162,4.50852949806831,7.99018735499102));
#16908=CARTESIAN_POINT('Ctrl Pts',(-5.37398699340618,4.99222544177309,8.0765322795457));
#16909=CARTESIAN_POINT('Ctrl Pts',(-5.99665145214228,5.1714851524102,8.16277826362009));
#16910=CARTESIAN_POINT('Ctrl Pts',(-6.61834156475152,4.99224641940564,8.24887393319591));
#16911=CARTESIAN_POINT('Ctrl Pts',(-7.03199547791655,4.52864873721892,8.33158922193082));
#16912=CARTESIAN_POINT('Ctrl Pts',(-7.1488251274158,3.94914585462493,8.4109047464235));
#16913=CARTESIAN_POINT('Ctrl Pts',(-6.98164895479995,3.4087990013883,8.48682398223609));
#16914=CARTESIAN_POINT('Ctrl Pts',(-6.61173888808033,3.04810158620894,8.55617610415385));
#16915=CARTESIAN_POINT('Ctrl Pts',(-6.17553818377882,2.89603620626052,8.61900861879084));
#16916=CARTESIAN_POINT('Ctrl Pts',(-5.7615552040565,2.91150440845813,8.67538071920882));
#16917=CARTESIAN_POINT('Ctrl Pts',(-5.38311467013871,3.07688868993499,8.73156698509197));
#16918=CARTESIAN_POINT('Ctrl Pts',(-5.0922662130037,3.3679196502838,8.78755020841222));
#16919=CARTESIAN_POINT('Ctrl Pts',(-4.92846880727788,3.74371374224587,8.84332192844384));
#16920=CARTESIAN_POINT('Ctrl Pts',(-4.9133631481404,4.15171775239193,8.89887160517648));
#16921=CARTESIAN_POINT('Ctrl Pts',(-5.04780408497372,4.5354318905722,8.95418932680646));
#16922=CARTESIAN_POINT('Ctrl Pts',(-5.3119896374796,4.84214892034485,9.00926581135202));
#16923=CARTESIAN_POINT('Ctrl Pts',(-5.66834727126242,5.03028402246597,9.06409240744499));
#16924=CARTESIAN_POINT('Ctrl Pts',(-6.06692750227203,5.07499815830979,9.11866109303675));
#16925=CARTESIAN_POINT('Ctrl Pts',(-6.45240069996794,4.97151173183086,9.17296460291645));
#16926=CARTESIAN_POINT('Ctrl Pts',(-6.77183253555119,4.73551241652737,9.22699618339229));
#16927=CARTESIAN_POINT('Ctrl Pts',(-6.98183516864551,4.40089583076875,9.28075020938804));
#16928=CARTESIAN_POINT('Ctrl Pts',(-7.05478648384277,4.01463129097058,9.33422085838521));
#16929=CARTESIAN_POINT('Ctrl Pts',(-6.98175677735204,3.63071267317424,9.38740512368169));
#16930=CARTESIAN_POINT('Ctrl Pts',(-6.75200291169346,3.26481365293951,9.4461747366418));
#16931=CARTESIAN_POINT('Ctrl Pts',(-6.34977481967191,3.0055454880072,9.51040222003417));
#16932=CARTESIAN_POINT('Ctrl Pts',(-5.83313933101808,2.96762824887196,9.57994102223053));
#16933=CARTESIAN_POINT('Ctrl Pts',(-5.34503066427212,3.18815853893367,9.65182587220209));
#16934=CARTESIAN_POINT('Ctrl Pts',(-5.02311880658278,3.64266389743902,9.72597672677365));
#16935=CARTESIAN_POINT('Ctrl Pts',(-4.99172936034754,4.21533123014454,9.80231318452775));
#16936=CARTESIAN_POINT('Ctrl Pts',(-5.26732576584318,4.71252690360499,9.87799134963007));
#16937=CARTESIAN_POINT('Ctrl Pts',(-5.76100357977955,4.98458611226293,9.95302302651522));
#16938=CARTESIAN_POINT('Ctrl Pts',(-6.3190068491534,4.95256557071688,10.0274239141637));
#16939=CARTESIAN_POINT('Ctrl Pts',(-6.77072516836847,4.63126492501222,10.1012133998304));
#16940=CARTESIAN_POINT('Ctrl Pts',(-6.98059479988593,4.12297966487163,10.1744145058383));
#16941=CARTESIAN_POINT('Ctrl Pts',(-6.88861527514656,3.58510760823276,10.2470537379492));
#16942=CARTESIAN_POINT('Ctrl Pts',(-6.52726164092553,3.18157524040098,10.3191609155057));
#16943=CARTESIAN_POINT('Ctrl Pts',(-6.01022182796172,3.03315029786899,10.3907690096979));
#16944=CARTESIAN_POINT('Ctrl Pts',(-5.4968023601685,3.18155424025962,10.4619139431723));
#16945=CARTESIAN_POINT('Ctrl Pts',(-5.14313043812835,3.57795790884971,10.5326343948435));
#16946=CARTESIAN_POINT('Ctrl Pts',(-5.05500749168914,4.09891712657135,10.6029715309616));
#16947=CARTESIAN_POINT('Ctrl Pts',(-5.25653896569849,4.58456546275314,10.6729687966083));
#16948=CARTESIAN_POINT('Ctrl Pts',(-5.68372978741289,4.88731233402227,10.7426716709992));
#16949=CARTESIAN_POINT('Ctrl Pts',(-6.20465835077419,4.91631905101284,10.812127333084));
#16950=CARTESIAN_POINT('Ctrl Pts',(-6.65989782842747,4.66449619813769,10.881384502152));
#16951=CARTESIAN_POINT('Ctrl Pts',(-6.91089426419046,4.21006249945785,10.9504928961986));
#16952=CARTESIAN_POINT('Ctrl Pts',(-6.88175267869527,3.69248340500686,11.0195035760517));
#16953=CARTESIAN_POINT('Ctrl Pts',(-6.58196495981473,3.26995322639814,11.0884671314299));
#16954=CARTESIAN_POINT('Ctrl Pts',(-6.10334225977061,3.07167484940034,11.1574367940911));
#16955=CARTESIAN_POINT('Ctrl Pts',(-5.59216302952149,3.15826911605838,11.2264605290878));
#16956=CARTESIAN_POINT('Ctrl Pts',(-5.2048518796542,3.50438369446588,11.295597623954));
#16957=CARTESIAN_POINT('Ctrl Pts',(-5.10870508884585,3.83722634528264,11.3417783904471));
#16958=CARTESIAN_POINT('Ctrl Pts',(-5.10868252218105,4.00485746418718,11.3649201584465));
#16959=CARTESIAN_POINT('Ctrl Pts',(-4.88818741853785,3.99652273593062,2.7252971556046));
#16960=CARTESIAN_POINT('Ctrl Pts',(-4.88821540189738,4.20439034906722,2.75399364169819));
#16961=CARTESIAN_POINT('Ctrl Pts',(-5.00770776252223,4.61848709275803,2.81144213686048));
#16962=CARTESIAN_POINT('Ctrl Pts',(-5.48915487885715,5.04852472807647,2.89735480549523));
#16963=CARTESIAN_POINT('Ctrl Pts',(-6.12369806164078,5.15592068267386,2.98303844498173));
#16964=CARTESIAN_POINT('Ctrl Pts',(-6.71613277769504,4.91015860270646,3.06841709492191));
#16965=CARTESIAN_POINT('Ctrl Pts',(-7.08548751283229,4.38888817555002,3.15345804613773));
#16966=CARTESIAN_POINT('Ctrl Pts',(-7.12071612532741,3.75390670031193,3.23811206508075));
#16967=CARTESIAN_POINT('Ctrl Pts',(-6.81423130553448,3.20031927366317,3.3223404682825));
#16968=CARTESIAN_POINT('Ctrl Pts',(-6.26324055802468,2.89636854220571,3.40610337940739));
#16969=CARTESIAN_POINT('Ctrl Pts',(-5.63875242508589,2.93197441766651,3.48936530830127));
#16970=CARTESIAN_POINT('Ctrl Pts',(-5.13221521099117,3.29207938503689,3.5720930071804));
#16971=CARTESIAN_POINT('Ctrl Pts',(-4.89655956374553,3.86258499488725,3.65425670745557));
#16972=CARTESIAN_POINT('Ctrl Pts',(-4.99982380419442,4.46664925394718,3.73582979403668));
#16973=CARTESIAN_POINT('Ctrl Pts',(-5.40561838084694,4.91973814590104,3.81678928615132));
#16974=CARTESIAN_POINT('Ctrl Pts',(-5.9856500350465,5.08614766178258,3.89711563403529));
#16975=CARTESIAN_POINT('Ctrl Pts',(-6.56076716216062,4.91979319813564,3.97679340115906));
#16976=CARTESIAN_POINT('Ctrl Pts',(-6.9409727052211,4.49304289155644,4.05288359943196));
#16977=CARTESIAN_POINT('Ctrl Pts',(-7.0474266977491,3.96276824766782,4.1254636569765));
#16978=CARTESIAN_POINT('Ctrl Pts',(-6.89516904973992,3.47063896532368,4.19460852763417));
#16979=CARTESIAN_POINT('Ctrl Pts',(-6.52878828735251,3.11405822440855,4.26322315390038));
#16980=CARTESIAN_POINT('Ctrl Pts',(-6.04039709877883,2.97684772888406,4.33130874407526));
#16981=CARTESIAN_POINT('Ctrl Pts',(-5.54968575410508,3.08960841211022,4.39887085217573));
#16982=CARTESIAN_POINT('Ctrl Pts',(-5.20683217278918,3.39296272348997,4.4603239618053));
#16983=CARTESIAN_POINT('Ctrl Pts',(-5.04409088312426,3.76709009322268,4.51582250927714));
#16984=CARTESIAN_POINT('Ctrl Pts',(-5.0305243603636,4.13190110393602,4.56548944357907));
#16985=CARTESIAN_POINT('Ctrl Pts',(-5.15069769713791,4.47444293139917,4.61488135084323));
#16986=CARTESIAN_POINT('Ctrl Pts',(-5.41235398803535,4.77868251941044,4.66946114941589));
#16987=CARTESIAN_POINT('Ctrl Pts',(-5.81774434138869,4.96115028608965,4.72912551946573));
#16988=CARTESIAN_POINT('Ctrl Pts',(-6.29798908339291,4.92457568437146,4.7937700973787));
#16989=CARTESIAN_POINT('Ctrl Pts',(-6.66628959161195,4.6862428401203,4.85262918959232));
#16990=CARTESIAN_POINT('Ctrl Pts',(-6.87368370032142,4.35485753503782,4.90584693774055));
#16991=CARTESIAN_POINT('Ctrl Pts',(-6.96176859520356,3.89555011703845,4.96941976954074));
#16992=CARTESIAN_POINT('Ctrl Pts',(-6.73846515358594,3.326843384695,5.04835438030133));
#16993=CARTESIAN_POINT('Ctrl Pts',(-6.08127895739378,3.01150227481938,5.14235131269286));
#16994=CARTESIAN_POINT('Ctrl Pts',(-5.39039177875388,3.22564211348055,5.23571232960406));
#16995=CARTESIAN_POINT('Ctrl Pts',(-5.03125804886121,3.84900889572268,5.32855013951349));
#16996=CARTESIAN_POINT('Ctrl Pts',(-5.19102205882783,4.54707913451127,5.42097217416568));
#16997=CARTESIAN_POINT('Ctrl Pts',(-5.78147777628547,4.9490719546746,5.51310246154377));
#16998=CARTESIAN_POINT('Ctrl Pts',(-6.32878590857654,4.86595140024166,5.58461352654982));
#16999=CARTESIAN_POINT('Ctrl Pts',(-6.62464558290292,4.64052456907037,5.63568596143666));
#17000=CARTESIAN_POINT('Ctrl Pts',(-6.8103718607247,4.408377865189,5.67654311110626));
#17001=CARTESIAN_POINT('Ctrl Pts',(-6.9227678104671,4.04462773784672,5.72760988707244));
#17002=CARTESIAN_POINT('Ctrl Pts',(-6.83202830824635,3.59672191844271,5.78895384400341));
#17003=CARTESIAN_POINT('Ctrl Pts',(-6.53801576444373,3.2459465336319,5.85036988114189));
#17004=CARTESIAN_POINT('Ctrl Pts',(-6.1112121268269,3.07843712584833,5.91191700931704));
#17005=CARTESIAN_POINT('Ctrl Pts',(-5.69297293187985,3.13080016207645,5.96847063433825));
#17006=CARTESIAN_POINT('Ctrl Pts',(-5.37267259566663,3.33259486980722,6.02002493947519));
#17007=CARTESIAN_POINT('Ctrl Pts',(-5.10046464604261,3.69910306117481,6.08205340782182));
#17008=CARTESIAN_POINT('Ctrl Pts',(-5.06292696992554,4.17870579852596,6.14434529872556));
#17009=CARTESIAN_POINT('Ctrl Pts',(-5.27983234324091,4.58585156841641,6.20696440567092));
#17010=CARTESIAN_POINT('Ctrl Pts',(-5.54182383632604,4.81195382016382,6.25410377148257));
#17011=CARTESIAN_POINT('Ctrl Pts',(-5.87037176036449,4.92684977784734,6.30142900406298));
#17012=CARTESIAN_POINT('Ctrl Pts',(-6.277665725455,4.912147013297,6.3568740012257));
#17013=CARTESIAN_POINT('Ctrl Pts',(-6.69688147273969,4.68142565956564,6.42058487897177));
#17014=CARTESIAN_POINT('Ctrl Pts',(-6.95983742269703,4.2067575540915,6.4927687132679));
#17015=CARTESIAN_POINT('Ctrl Pts',(-6.93454926747412,3.7524263987416,6.55336958191222));
#17016=CARTESIAN_POINT('Ctrl Pts',(-6.77094221790365,3.43645100527889,6.60213705006757));
#17017=CARTESIAN_POINT('Ctrl Pts',(-6.56675769701475,3.22009853002638,6.64293797584287));
#17018=CARTESIAN_POINT('Ctrl Pts',(-6.27376286057791,3.06500756365233,6.68803045805404));
#17019=CARTESIAN_POINT('Ctrl Pts',(-5.91262828551806,3.02417323682573,6.7374938299492));
#17020=CARTESIAN_POINT('Ctrl Pts',(-5.50041955363556,3.13401397168084,6.79552405315717));
#17021=CARTESIAN_POINT('Ctrl Pts',(-5.12579134765909,3.46752514898312,6.86231607408146));
#17022=CARTESIAN_POINT('Ctrl Pts',(-4.96753625041387,4.0146614836518,6.93810751304089));
#17023=CARTESIAN_POINT('Ctrl Pts',(-5.1258462367197,4.56667432610493,7.01456115074844));
#17024=CARTESIAN_POINT('Ctrl Pts',(-5.55738945542098,4.95330479961627,7.09168401731796));
#17025=CARTESIAN_POINT('Ctrl Pts',(-6.13343345309169,5.0518789878103,7.16947953573716));
#17026=CARTESIAN_POINT('Ctrl Pts',(-6.67830016319192,4.82695811831511,7.24794698514151));
#17027=CARTESIAN_POINT('Ctrl Pts',(-7.02287341594567,4.34252758285008,7.32708173585149));
#17028=CARTESIAN_POINT('Ctrl Pts',(-7.05716836822738,3.74409198272662,7.40687517558502));
#17029=CARTESIAN_POINT('Ctrl Pts',(-6.76546001393813,3.21489650644473,7.48731481614497));
#17030=CARTESIAN_POINT('Ctrl Pts',(-6.23276792464148,2.91974253368875,7.56838433004706));
#17031=CARTESIAN_POINT('Ctrl Pts',(-5.62012631091812,2.95351650439889,7.6500636810307));
#17032=CARTESIAN_POINT('Ctrl Pts',(-5.11578092937486,3.31062596268586,7.73232921118835));
#17033=CARTESIAN_POINT('Ctrl Pts',(-4.87716301346901,3.88521462852368,7.81515385688724));
#17034=CARTESIAN_POINT('Ctrl Pts',(-4.98150003080198,4.50259039415197,7.89850713183724));
#17035=CARTESIAN_POINT('Ctrl Pts',(-5.40084975729399,4.97257222017584,7.98235571360354));
#17036=CARTESIAN_POINT('Ctrl Pts',(-6.00920307899455,5.1483232714495,8.06666278343668));
#17037=CARTESIAN_POINT('Ctrl Pts',(-6.62101815995564,4.97255948752676,8.15139018914161));
#17038=CARTESIAN_POINT('Ctrl Pts',(-7.031197198535,4.5137306423188,8.23334232564202));
#17039=CARTESIAN_POINT('Ctrl Pts',(-7.14810753526542,3.93609131852819,8.31243675863358));
#17040=CARTESIAN_POINT('Ctrl Pts',(-6.98085185281347,3.39401206249462,8.38858984271055));
#17041=CARTESIAN_POINT('Ctrl Pts',(-6.60786439273102,3.0297840906944,8.45858050620251));
#17042=CARTESIAN_POINT('Ctrl Pts',(-6.16543932526409,2.87532757953747,8.5223305258315));
#17043=CARTESIAN_POINT('Ctrl Pts',(-5.74360228126044,2.8909186429676,8.57978397402559));
#17044=CARTESIAN_POINT('Ctrl Pts',(-5.35620785573692,3.06001727071349,8.63729389811813));
#17045=CARTESIAN_POINT('Ctrl Pts',(-5.05708743686595,3.35908200537455,8.69485647369181));
#17046=CARTESIAN_POINT('Ctrl Pts',(-4.88780606075004,3.74701902455501,8.75245114704132));
#17047=CARTESIAN_POINT('Ctrl Pts',(-4.87196989522485,4.1700891625295,8.81006291512397));
#17048=CARTESIAN_POINT('Ctrl Pts',(-5.0118054178791,4.56971615713679,8.8676763948023));
#17049=CARTESIAN_POINT('Ctrl Pts',(-5.28792248480184,4.890542511533,8.92527629977779));
#17050=CARTESIAN_POINT('Ctrl Pts',(-5.66198182516304,5.08820876432408,8.98284725651621));
#17051=CARTESIAN_POINT('Ctrl Pts',(-6.0820877117984,5.13549890117965,9.04037419150282));
#17052=CARTESIAN_POINT('Ctrl Pts',(-6.49000316987433,5.02614937727024,9.09784167889789));
#17053=CARTESIAN_POINT('Ctrl Pts',(-6.82935485126433,4.77562168586658,9.15523548794978));
#17054=CARTESIAN_POINT('Ctrl Pts',(-7.05332363279532,4.41902744506835,9.212539258798));
#17055=CARTESIAN_POINT('Ctrl Pts',(-7.13149777824104,4.0058899312146,9.26974207432468));
#17056=CARTESIAN_POINT('Ctrl Pts',(-7.05325025901744,3.59384616685398,9.32682158392224));
#17057=CARTESIAN_POINT('Ctrl Pts',(-6.80601788545062,3.19983310992077,9.39010187571138));
#17058=CARTESIAN_POINT('Ctrl Pts',(-6.37157118006669,2.91948826298353,9.45950184637294));
#17059=CARTESIAN_POINT('Ctrl Pts',(-5.81129742273106,2.87811150813228,9.53491939436006));
#17060=CARTESIAN_POINT('Ctrl Pts',(-5.28002903323734,3.11786749908228,9.61315039744257));
#17061=CARTESIAN_POINT('Ctrl Pts',(-4.9283350120672,3.6139208970815,9.69411146456086));
#17062=CARTESIAN_POINT('Ctrl Pts',(-4.89370159918598,4.24102415054889,9.77770799761992));
#17063=CARTESIAN_POINT('Ctrl Pts',(-5.19607987629306,4.78697274776535,9.86079177231777));
#17064=CARTESIAN_POINT('Ctrl Pts',(-5.73907951104547,5.08640154454074,9.94333062311419));
#17065=CARTESIAN_POINT('Ctrl Pts',(-6.35384370981652,5.05124052418518,10.0252959393708));
#17066=CARTESIAN_POINT('Ctrl Pts',(-6.85201199676228,4.69698298891633,10.1066623538334));
#17067=CARTESIAN_POINT('Ctrl Pts',(-7.08354537291699,4.13627475394443,10.1874080858196));
#17068=CARTESIAN_POINT('Ctrl Pts',(-6.98206739002019,3.54305655090038,10.2675149918412));
#17069=CARTESIAN_POINT('Ctrl Pts',(-6.58379031327503,3.09841677074597,10.3469687190531));
#17070=CARTESIAN_POINT('Ctrl Pts',(-6.01478263762881,2.93521361028816,10.4257587680015));
#17071=CARTESIAN_POINT('Ctrl Pts',(-5.45099736693054,3.09836839685132,10.5038785653285));
#17072=CARTESIAN_POINT('Ctrl Pts',(-5.06379832767988,3.53270296534894,10.5813254926886));
#17073=CARTESIAN_POINT('Ctrl Pts',(-4.96787158020713,4.10149828156937,10.6581009257139));
#17074=CARTESIAN_POINT('Ctrl Pts',(-5.18734967510211,4.62953051145273,10.7342101718087));
#17075=CARTESIAN_POINT('Ctrl Pts',(-5.65009570631128,4.9570153326714,10.8096625555231));
#17076=CARTESIAN_POINT('Ctrl Pts',(-6.21132939882819,4.98785053970112,10.8844711049253));
#17077=CARTESIAN_POINT('Ctrl Pts',(-6.69884790173685,4.71765887213222,10.9586530325065));
#17078=CARTESIAN_POINT('Ctrl Pts',(-6.96572373527273,4.23348678541994,11.0322283773605));
#17079=CARTESIAN_POINT('Ctrl Pts',(-6.93439113090648,3.68591170270209,11.1052227079854));
#17080=CARTESIAN_POINT('Ctrl Pts',(-6.61898532491596,3.24226468152419,11.177660612388));
#17081=CARTESIAN_POINT('Ctrl Pts',(-6.11957413084598,3.03597618734333,11.2495797434453));
#17082=CARTESIAN_POINT('Ctrl Pts',(-5.59059433608062,3.12614738105264,11.3209988490037));
#17083=CARTESIAN_POINT('Ctrl Pts',(-5.19328964279077,3.48207627459039,11.391988770315));
#17084=CARTESIAN_POINT('Ctrl Pts',(-5.09580204375325,3.8211227121471,11.4389948522726));
#17085=CARTESIAN_POINT('Ctrl Pts',(-5.09577912292024,3.99138468562821,11.4624998143295));
#17086=CARTESIAN_POINT('Ctrl Pts',(-4.91064567402416,4.00976796878862,2.62933128061604));
#17087=CARTESIAN_POINT('Ctrl Pts',(-4.91067314116014,4.21380094025299,2.65749838774693));
#17088=CARTESIAN_POINT('Ctrl Pts',(-5.02777738329904,4.62104843715925,2.71397001944354));
#17089=CARTESIAN_POINT('Ctrl Pts',(-5.50410058883396,5.04740518005545,2.79904516502667));
#17090=CARTESIAN_POINT('Ctrl Pts',(-6.13662098078803,5.15502614256399,2.8844538444374));
#17091=CARTESIAN_POINT('Ctrl Pts',(-6.73153984852692,4.90888416817942,2.97014996728053));
#17092=CARTESIAN_POINT('Ctrl Pts',(-7.10531686090369,4.3823820288213,3.05608627462904));
#17093=CARTESIAN_POINT('Ctrl Pts',(-7.14175290484821,3.73630540538697,3.14221378953781));
#17094=CARTESIAN_POINT('Ctrl Pts',(-6.82832380401177,3.16895406741704,3.2284825451846));
#17095=CARTESIAN_POINT('Ctrl Pts',(-6.26048494912823,2.85504067087679,3.31484168882952));
#17096=CARTESIAN_POINT('Ctrl Pts',(-5.61239401723101,2.8914159142622,3.40123983352415));
#17097=CARTESIAN_POINT('Ctrl Pts',(-5.08310915284364,3.26700614953085,3.48762540366753));
#17098=CARTESIAN_POINT('Ctrl Pts',(-4.83502303080036,3.86619292249913,3.57394686629917));
#17099=CARTESIAN_POINT('Ctrl Pts',(-4.94364485875093,4.50465820699671,3.66015309210022));
#17100=CARTESIAN_POINT('Ctrl Pts',(-5.37453858626572,4.98650442879576,3.74619359342917));
#17101=CARTESIAN_POINT('Ctrl Pts',(-5.99413141917538,5.16474071398009,3.83201900827667));
#17102=CARTESIAN_POINT('Ctrl Pts',(-6.61181106100534,4.98652297157529,3.91758092543883));
#17103=CARTESIAN_POINT('Ctrl Pts',(-7.02227060414855,4.5263763294177,3.99967575252517));
#17104=CARTESIAN_POINT('Ctrl Pts',(-7.13784103488286,3.95201571751744,4.07830186066915));
#17105=CARTESIAN_POINT('Ctrl Pts',(-6.97254187154243,3.41698947452407,4.15347334639407));
#17106=CARTESIAN_POINT('Ctrl Pts',(-6.57314391987666,3.02798986662469,4.22830470821497));
#17107=CARTESIAN_POINT('Ctrl Pts',(-6.03910362822948,2.87777890366138,4.30276940850961));
#17108=CARTESIAN_POINT('Ctrl Pts',(-5.50111638215199,3.00124361271675,4.37684151437551));
#17109=CARTESIAN_POINT('Ctrl Pts',(-5.12440677043376,3.33442645158616,4.44436384283435));
#17110=CARTESIAN_POINT('Ctrl Pts',(-4.94533142154725,3.74599828483902,4.50542710461716));
#17111=CARTESIAN_POINT('Ctrl Pts',(-4.93036487906514,4.14774216402424,4.56013064511645));
#17112=CARTESIAN_POINT('Ctrl Pts',(-5.06278625695976,4.52525542320837,4.61457215171803));
#17113=CARTESIAN_POINT('Ctrl Pts',(-5.35129270421363,4.86073725652708,4.67476507190189));
#17114=CARTESIAN_POINT('Ctrl Pts',(-5.79842815503293,5.06199857300563,4.74058481530442));
#17115=CARTESIAN_POINT('Ctrl Pts',(-6.32805210185099,5.02164378663595,4.81188343610946));
#17116=CARTESIAN_POINT('Ctrl Pts',(-6.73397836813742,4.75890073365287,4.87677640400761));
#17117=CARTESIAN_POINT('Ctrl Pts',(-6.96231833364606,4.39398026117723,4.93538713836827));
#17118=CARTESIAN_POINT('Ctrl Pts',(-7.05915977358153,3.88872695911014,5.00532566139195));
#17119=CARTESIAN_POINT('Ctrl Pts',(-6.81364543951855,3.26450858713251,5.09201750919447));
#17120=CARTESIAN_POINT('Ctrl Pts',(-6.09460099291618,2.92021072923617,5.19484760834442));
#17121=CARTESIAN_POINT('Ctrl Pts',(-5.34288634734843,3.15403642928638,5.29649459932079));
#17122=CARTESIAN_POINT('Ctrl Pts',(-4.95511179166806,3.82898994813764,5.39697466684311));
#17123=CARTESIAN_POINT('Ctrl Pts',(-5.12784877934483,4.5789002529021,5.49632431032147));
#17124=CARTESIAN_POINT('Ctrl Pts',(-5.75808193491375,5.00652139410731,5.59458312904311));
#17125=CARTESIAN_POINT('Ctrl Pts',(-6.33648847978147,4.9176997738217,5.67021042750851));
#17126=CARTESIAN_POINT('Ctrl Pts',(-6.64717042016579,4.68086196158556,5.7238634266878));
#17127=CARTESIAN_POINT('Ctrl Pts',(-6.8416021768888,4.4377454131655,5.7666459073939));
#17128=CARTESIAN_POINT('Ctrl Pts',(-6.95838649841976,4.05859511388473,5.81987849038407));
#17129=CARTESIAN_POINT('Ctrl Pts',(-6.86409262477757,3.59516210271433,5.88336519673482));
#17130=CARTESIAN_POINT('Ctrl Pts',(-6.56159285132325,3.23491908721871,5.94650414310894));
#17131=CARTESIAN_POINT('Ctrl Pts',(-6.12597096392956,3.06439414322808,6.0093074876293));
#17132=CARTESIAN_POINT('Ctrl Pts',(-5.70236686608432,3.1178198313833,6.0666074274623));
#17133=CARTESIAN_POINT('Ctrl Pts',(-5.380122673147,3.32104386243891,6.11850003188511));
#17134=CARTESIAN_POINT('Ctrl Pts',(-5.10787632083129,3.68804825140651,6.18058621464548));
#17135=CARTESIAN_POINT('Ctrl Pts',(-5.07150998975464,4.16419512411157,6.24242799659425));
#17136=CARTESIAN_POINT('Ctrl Pts',(-5.28523589548665,4.56477917688274,6.30407580547538));
#17137=CARTESIAN_POINT('Ctrl Pts',(-5.54182678085649,4.78602928247548,6.35023001525522));
#17138=CARTESIAN_POINT('Ctrl Pts',(-5.86180686221491,4.89774513429516,6.39631824503907));
#17139=CARTESIAN_POINT('Ctrl Pts',(-6.25632381243741,4.88331058519368,6.45002738837586));
#17140=CARTESIAN_POINT('Ctrl Pts',(-6.65956563830335,4.66083856383486,6.51135090062564));
#17141=CARTESIAN_POINT('Ctrl Pts',(-6.91027780675986,4.20716380710425,6.58030861757756));
#17142=CARTESIAN_POINT('Ctrl Pts',(-6.88590244429634,3.77627762225862,6.63779205741682));
#17143=CARTESIAN_POINT('Ctrl Pts',(-6.73144725053243,3.47814458537331,6.68381436763788));
#17144=CARTESIAN_POINT('Ctrl Pts',(-6.53934056134022,3.27467116868115,6.72219376697843));
#17145=CARTESIAN_POINT('Ctrl Pts',(-6.26469099012521,3.12942239607942,6.76445537433218));
#17146=CARTESIAN_POINT('Ctrl Pts',(-5.92756071018149,3.09141899259667,6.81062906476635));
#17147=CARTESIAN_POINT('Ctrl Pts',(-5.54422762795656,3.19370614855236,6.86459746291479));
#17148=CARTESIAN_POINT('Ctrl Pts',(-5.19754383461621,3.50275475425966,6.92643961530437));
#17149=CARTESIAN_POINT('Ctrl Pts',(-5.05200826635028,4.00707808463828,6.99628451388278));
#17150=CARTESIAN_POINT('Ctrl Pts',(-5.19756546451278,4.51362930224783,7.06644704414763));
#17151=CARTESIAN_POINT('Ctrl Pts',(-5.59238323965525,4.86704223287948,7.13697216632295));
#17152=CARTESIAN_POINT('Ctrl Pts',(-6.11767746247401,4.95673943944794,7.20790194100564));
#17153=CARTESIAN_POINT('Ctrl Pts',(-6.61329771063287,4.75199100760384,7.27927638914268));
#17154=CARTESIAN_POINT('Ctrl Pts',(-6.92614139128033,4.31199654687507,7.35113275685342));
#17155=CARTESIAN_POINT('Ctrl Pts',(-6.9571975467719,3.76912800444529,7.423505503059));
#17156=CARTESIAN_POINT('Ctrl Pts',(-6.69270421729341,3.28932324733122,7.49642599103587));
#17157=CARTESIAN_POINT('Ctrl Pts',(-6.20970313639906,3.02166164921741,7.56992237489679));
#17158=CARTESIAN_POINT('Ctrl Pts',(-5.65382074027343,3.05222706591483,7.6440193764838));
#17159=CARTESIAN_POINT('Ctrl Pts',(-5.19557577726472,3.37654361855234,7.71873817781238));
#17160=CARTESIAN_POINT('Ctrl Pts',(-4.97826782350353,3.8993856502534,7.79409623237114));
#17161=CARTESIAN_POINT('Ctrl Pts',(-5.07323032347364,4.46254478708333,7.8701072988587));
#17162=CARTESIAN_POINT('Ctrl Pts',(-5.45660461493641,4.89258443960897,7.94678104764465));
#17163=CARTESIAN_POINT('Ctrl Pts',(-6.01476043904619,5.05413520603182,8.02412366366451));
#17164=CARTESIAN_POINT('Ctrl Pts',(-6.57833417536576,4.89257846081219,8.10213633415574));
#17165=CARTESIAN_POINT('Ctrl Pts',(-6.95791455951021,4.46849196311221,8.17790431988503));
#17166=CARTESIAN_POINT('Ctrl Pts',(-7.06677953585924,3.93210458538223,8.25133598903447));
#17167=CARTESIAN_POINT('Ctrl Pts',(-6.91104997509509,3.42641897107069,8.32235387143313));
#17168=CARTESIAN_POINT('Ctrl Pts',(-6.56180003391545,3.08496284345591,8.38791761690604));
#17169=CARTESIAN_POINT('Ctrl Pts',(-6.1456027543353,2.93950056003664,8.44788090837857));
#17170=CARTESIAN_POINT('Ctrl Pts',(-5.74726494655331,2.95408057114023,8.50212056041012));
#17171=CARTESIAN_POINT('Ctrl Pts',(-5.37997347796744,3.11424831925692,8.55663140495941));
#17172=CARTESIAN_POINT('Ctrl Pts',(-5.09521302131359,3.398741500323,8.61139836356879));
#17173=CARTESIAN_POINT('Ctrl Pts',(-4.93332872853029,3.76934469312497,8.66641734559057));
#17174=CARTESIAN_POINT('Ctrl Pts',(-4.91797985132647,4.17523812948246,8.72167965701057));
#17175=CARTESIAN_POINT('Ctrl Pts',(-5.05255498515063,4.56031052428824,8.77717618865606));
#17176=CARTESIAN_POINT('Ctrl Pts',(-5.31959588340143,4.87083760394284,8.8328971565062));
#17177=CARTESIAN_POINT('Ctrl Pts',(-5.68301975204626,5.06306855289482,8.8888322510767));
#17178=CARTESIAN_POINT('Ctrl Pts',(-6.09304345640864,5.10939106913153,8.9449704650885));
#17179=CARTESIAN_POINT('Ctrl Pts',(-6.49299926542453,5.00234860987632,9.0013005551928));
#17180=CARTESIAN_POINT('Ctrl Pts',(-6.82728558123996,4.75577359118481,9.05781010687818));
#17181=CARTESIAN_POINT('Ctrl Pts',(-7.04898193413433,4.40311250625515,9.11448771824764));
#17182=CARTESIAN_POINT('Ctrl Pts',(-7.12683472133885,3.99261902493127,9.17131822613187));
#17183=CARTESIAN_POINT('Ctrl Pts',(-7.04888849326792,3.58126093676225,9.22829351281217));
#17184=CARTESIAN_POINT('Ctrl Pts',(-6.80115336644072,3.18607404321642,9.29173806496654));
#17185=CARTESIAN_POINT('Ctrl Pts',(-6.36340806671669,2.90314134363089,9.36168982415459));
#17186=CARTESIAN_POINT('Ctrl Pts',(-5.79521809157173,2.86076218208454,9.43817009255432));
#17187=CARTESIAN_POINT('Ctrl Pts',(-5.25303743345012,3.10496561424916,9.51797381367612));
#17188=CARTESIAN_POINT('Ctrl Pts',(-4.89152375820551,3.61390066850146,9.60108189482633));
#17189=CARTESIAN_POINT('Ctrl Pts',(-4.85515441846885,4.26189522592992,9.68745972603124));
#17190=CARTESIAN_POINT('Ctrl Pts',(-5.16913161772041,4.82994539286161,9.77385897203761));
#17191=CARTESIAN_POINT('Ctrl Pts',(-5.73709448115372,5.14376652967341,9.86022814221491));
#17192=CARTESIAN_POINT('Ctrl Pts',(-6.38432934899975,5.10727832815486,9.94651569088689));
#17193=CARTESIAN_POINT('Ctrl Pts',(-6.91211582322222,4.73257940117262,10.0326707058309));
#17194=CARTESIAN_POINT('Ctrl Pts',(-7.15907764199467,4.13576450802929,10.1186429904321));
#17195=CARTESIAN_POINT('Ctrl Pts',(-7.05090943421799,3.50076864306298,10.2043834497604));
#17196=CARTESIAN_POINT('Ctrl Pts',(-6.62285029522974,3.0222538279605,10.2898443693623));
#17197=CARTESIAN_POINT('Ctrl Pts',(-6.00816185318676,2.84554979076536,10.3749796891461));
#17198=CARTESIAN_POINT('Ctrl Pts',(-5.39636640563317,3.02223735184074,10.4597452748207));
#17199=CARTESIAN_POINT('Ctrl Pts',(-4.97444631827297,3.49505631224499,10.5440991603088));
#17200=CARTESIAN_POINT('Ctrl Pts',(-4.86936219074472,4.11653834401228,10.6280018501589));
#17201=CARTESIAN_POINT('Ctrl Pts',(-5.10966657939444,4.69526291176007,10.7114164772727));
#17202=CARTESIAN_POINT('Ctrl Pts',(-5.61786112599645,5.05513200621197,10.7943090970552));
#17203=CARTESIAN_POINT('Ctrl Pts',(-6.23548062728098,5.08919687074565,10.8766487583371));
#17204=CARTESIAN_POINT('Ctrl Pts',(-6.77273351761296,4.79153197079639,10.9584079804219));
#17205=CARTESIAN_POINT('Ctrl Pts',(-7.06706144191725,4.25760734730938,11.0395622358401));
#17206=CARTESIAN_POINT('Ctrl Pts',(-7.03247204506743,3.65362797051252,11.1200915649221));
#17207=CARTESIAN_POINT('Ctrl Pts',(-6.68464073545661,3.16451872129078,11.1999774348503));
#17208=CARTESIAN_POINT('Ctrl Pts',(-6.13448705150615,2.9373955420016,11.2792100819558));
#17209=CARTESIAN_POINT('Ctrl Pts',(-5.55274917991616,3.03673746832776,11.3577723501083));
#17210=CARTESIAN_POINT('Ctrl Pts',(-5.11690626681905,3.42739822280303,11.4356762391777));
#17211=CARTESIAN_POINT('Ctrl Pts',(-5.01030553006867,3.79852727230778,11.4871434418717));
#17212=CARTESIAN_POINT('Ctrl Pts',(-5.01028050391396,3.98442812877985,11.5128073789705));
#17213=CARTESIAN_POINT('Ctrl Pts',(-4.97008191124374,4.01367950132792,2.60093950625076));
#17214=CARTESIAN_POINT('Ctrl Pts',(-4.97010792325056,4.20690339805964,2.62761440178568));
#17215=CARTESIAN_POINT('Ctrl Pts',(-5.08093760858241,4.59266080489006,2.68110100679445));
#17216=CARTESIAN_POINT('Ctrl Pts',(-5.53326658633966,4.99790615693166,2.76192472631994));
#17217=CARTESIAN_POINT('Ctrl Pts',(-6.13586869185039,5.10068577095782,2.84329383983683));
#17218=CARTESIAN_POINT('Ctrl Pts',(-6.7045933205602,4.86571328724988,2.92519942604245));
#17219=CARTESIAN_POINT('Ctrl Pts',(-7.06331496787067,4.36097514622367,3.00761019396623));
#17220=CARTESIAN_POINT('Ctrl Pts',(-7.0987250270912,3.73918273690758,3.09050050603284));
#17221=CARTESIAN_POINT('Ctrl Pts',(-6.79624457301434,3.19090820274708,3.17383813798714));
#17222=CARTESIAN_POINT('Ctrl Pts',(-6.24569553319637,2.88613001714052,3.25758997671661));
#17223=CARTESIAN_POINT('Ctrl Pts',(-5.61454866908592,2.92117214212433,3.34171971865797));
#17224=CARTESIAN_POINT('Ctrl Pts',(-5.09672508083302,3.28814927637395,3.4261891931306));
#17225=CARTESIAN_POINT('Ctrl Pts',(-4.8527010496301,3.87647815686147,3.51095811781651));
#17226=CARTESIAN_POINT('Ctrl Pts',(-4.95944840393067,4.50636398239007,3.595984371598));
#17227=CARTESIAN_POINT('Ctrl Pts',(-5.38609475348018,4.98408471257233,3.68122458091311));
#17228=CARTESIAN_POINT('Ctrl Pts',(-6.00268079420748,5.16189327329318,3.76663345374862));
#17229=CARTESIAN_POINT('Ctrl Pts',(-6.62039054353995,4.98411118093899,3.85216610920168));
#17230=CARTESIAN_POINT('Ctrl Pts',(-7.03296634594375,4.52220299265115,3.93460295352821));
#17231=CARTESIAN_POINT('Ctrl Pts',(-7.14985065007003,3.94288654783804,4.01389927783044));
#17232=CARTESIAN_POINT('Ctrl Pts',(-6.98272205096131,3.40093752568897,4.0900113004944));
#17233=CARTESIAN_POINT('Ctrl Pts',(-6.57680875018895,3.00520046094579,4.16608365584876));
#17234=CARTESIAN_POINT('Ctrl Pts',(-6.03173171378752,2.85157669802245,4.24208403850743));
#17235=CARTESIAN_POINT('Ctrl Pts',(-5.48034738502237,2.97784080438086,4.31797832595391));
#17236=CARTESIAN_POINT('Ctrl Pts',(-5.09268849546396,3.32036229583066,4.3874112267225));
#17237=CARTESIAN_POINT('Ctrl Pts',(-4.90777324710137,3.74504999230099,4.45041329672765));
#17238=CARTESIAN_POINT('Ctrl Pts',(-4.89217896507905,4.16075012922992,4.50700493335702));
#17239=CARTESIAN_POINT('Ctrl Pts',(-5.02947267525229,4.55245617462658,4.56347581988345));
#17240=CARTESIAN_POINT('Ctrl Pts',(-5.32947452049713,4.90147627896693,4.62607044249519));
#17241=CARTESIAN_POINT('Ctrl Pts',(-5.79584535398848,5.11161943763673,4.69471754610501));
#17242=CARTESIAN_POINT('Ctrl Pts',(-6.35014451448374,5.06959102637412,4.7693250241412));
#17243=CARTESIAN_POINT('Ctrl Pts',(-6.77631798822209,4.79395495836344,4.83741703394908));
#17244=CARTESIAN_POINT('Ctrl Pts',(-7.01666455556856,4.40998698374066,4.89908002516321));
#17245=CARTESIAN_POINT('Ctrl Pts',(-7.11887670267137,3.87728204193206,4.97281129786051));
#17246=CARTESIAN_POINT('Ctrl Pts',(-6.85969875513886,3.21712465631829,5.06443234656144));
#17247=CARTESIAN_POINT('Ctrl Pts',(-6.09709548778395,2.85143338377357,5.17348766082218));
#17248=CARTESIAN_POINT('Ctrl Pts',(-5.29731395843599,3.09982709410499,5.28157901580182));
#17249=CARTESIAN_POINT('Ctrl Pts',(-4.88367792874778,3.81923523883344,5.38866556777043));
#17250=CARTESIAN_POINT('Ctrl Pts',(-5.06792313288877,4.61994565311358,5.49470491264318));
#17251=CARTESIAN_POINT('Ctrl Pts',(-5.74134532638002,5.07694585878306,5.59967630177535));
#17252=CARTESIAN_POINT('Ctrl Pts',(-6.35946722683167,4.98198830174697,5.68046971855626));
#17253=CARTESIAN_POINT('Ctrl Pts',(-6.69137247180265,4.72895391359148,5.7377846585707));
#17254=CARTESIAN_POINT('Ctrl Pts',(-6.89903102024635,4.46928826285102,5.78347589255367));
#17255=CARTESIAN_POINT('Ctrl Pts',(-7.02364136198497,4.06457023003713,5.84028303985189));
#17256=CARTESIAN_POINT('Ctrl Pts',(-6.92300892708766,3.5704067168229,5.90797894643917));
#17257=CARTESIAN_POINT('Ctrl Pts',(-6.60082158074705,3.18688178295313,5.97519979799271));
#17258=CARTESIAN_POINT('Ctrl Pts',(-6.13768958587062,3.00572129709394,6.04195922782834));
#17259=CARTESIAN_POINT('Ctrl Pts',(-5.6883298773806,3.06253696090835,6.10274000217679));
#17260=CARTESIAN_POINT('Ctrl Pts',(-5.34722099251186,3.27774259824664,6.15767505319115));
#17261=CARTESIAN_POINT('Ctrl Pts',(-5.0596350596403,3.66561735956058,6.22327451214416));
#17262=CARTESIAN_POINT('Ctrl Pts',(-5.02173651226817,4.16716900833336,6.28840828372746));
#17263=CARTESIAN_POINT('Ctrl Pts',(-5.24614992976449,4.58745247284312,6.35310163465723));
#17264=CARTESIAN_POINT('Ctrl Pts',(-5.51477848997985,4.81896891835744,6.40141121346934));
#17265=CARTESIAN_POINT('Ctrl Pts',(-5.84881374774272,4.9354787272431,6.4495201665249));
#17266=CARTESIAN_POINT('Ctrl Pts',(-6.25943186378334,4.92033084311256,6.50542267537317));
#17267=CARTESIAN_POINT('Ctrl Pts',(-6.67740663203018,4.68935725087564,6.56901532400741));
#17268=CARTESIAN_POINT('Ctrl Pts',(-6.93578121619537,4.22100070878716,6.64018116904655));
#17269=CARTESIAN_POINT('Ctrl Pts',(-6.9104300619441,3.77859534030824,6.699213603944));
#17270=CARTESIAN_POINT('Ctrl Pts',(-6.75240590109235,3.47372741247044,6.74628509889055));
#17271=CARTESIAN_POINT('Ctrl Pts',(-6.55640934718448,3.26621135700427,6.78543648927768));
#17272=CARTESIAN_POINT('Ctrl Pts',(-6.27707437535794,3.11861349905881,6.82841657096604));
#17273=CARTESIAN_POINT('Ctrl Pts',(-5.9355022847588,3.08022875183803,6.87520052017041));
#17274=CARTESIAN_POINT('Ctrl Pts',(-5.54858200380153,3.1836250601501,6.92968354415467));
#17275=CARTESIAN_POINT('Ctrl Pts',(-5.20045972734387,3.49445659550131,6.99184374671821));
#17276=CARTESIAN_POINT('Ctrl Pts',(-5.05544732191987,3.99851041473827,7.06165119985256));
#17277=CARTESIAN_POINT('Ctrl Pts',(-5.20048107826059,4.50175960678276,7.13139174737956));
#17278=CARTESIAN_POINT('Ctrl Pts',(-5.59093790031351,4.85072254510397,7.20110862526653));
#17279=CARTESIAN_POINT('Ctrl Pts',(-6.10734774732503,4.93850031945277,7.27085082830924));
#17280=CARTESIAN_POINT('Ctrl Pts',(-6.59183509574101,4.7379341695227,7.34066464130002));
#17281=CARTESIAN_POINT('Ctrl Pts',(-6.89590284323148,4.30964148274272,7.41059704126021));
#17282=CARTESIAN_POINT('Ctrl Pts',(-6.92561924919337,3.78399509029939,7.48069377094016));
#17283=CARTESIAN_POINT('Ctrl Pts',(-6.6704002715619,3.32170621392155,7.5509998057238));
#17284=CARTESIAN_POINT('Ctrl Pts',(-6.20670653876933,3.06509997300355,7.62155879348131));
#17285=CARTESIAN_POINT('Ctrl Pts',(-5.67534724500118,3.09460421450561,7.69241293056779));
#17286=CARTESIAN_POINT('Ctrl Pts',(-5.23904547633351,3.40371059691615,7.76360262044568));
#17287=CARTESIAN_POINT('Ctrl Pts',(-5.0329663099472,3.90014632476456,7.83516634990396));
#17288=CARTESIAN_POINT('Ctrl Pts',(-5.12305877544344,4.43317697771956,7.90714029938048));
#17289=CARTESIAN_POINT('Ctrl Pts',(-5.48516295948042,4.83908746429057,7.97955849057881));
#17290=CARTESIAN_POINT('Ctrl Pts',(-6.01107465918283,4.99114822692247,8.05245176655152));
#17291=CARTESIAN_POINT('Ctrl Pts',(-6.54108875049124,4.83908239809763,8.1258494812478));
#17292=CARTESIAN_POINT('Ctrl Pts',(-6.89755173489568,4.44070311733813,8.19703730133364));
#17293=CARTESIAN_POINT('Ctrl Pts',(-6.99966563994677,3.93733853721186,8.26597111831699));
#17294=CARTESIAN_POINT('Ctrl Pts',(-6.8536012652616,3.46307615160578,8.33258743659512));
#17295=CARTESIAN_POINT('Ctrl Pts',(-6.52611138411337,3.14291249345024,8.39407543281095));
#17296=CARTESIAN_POINT('Ctrl Pts',(-6.13582853537318,3.00649193719368,8.45031886967759));
#17297=CARTESIAN_POINT('Ctrl Pts',(-5.76220105188843,3.02015704448408,8.50120517126138));
#17298=CARTESIAN_POINT('Ctrl Pts',(-5.41757335971822,3.17041692695101,8.55235642674854));
#17299=CARTESIAN_POINT('Ctrl Pts',(-5.15021641590212,3.43748811582643,8.60378222122026));
#17300=CARTESIAN_POINT('Ctrl Pts',(-4.99809986343188,3.78564552616636,8.65547998995423));
#17301=CARTESIAN_POINT('Ctrl Pts',(-4.98362774422425,4.16729388058725,8.70744993309881));
#17302=CARTESIAN_POINT('Ctrl Pts',(-5.11024697508206,4.52974174117404,8.75969162933513));
#17303=CARTESIAN_POINT('Ctrl Pts',(-5.36183465340263,4.82237913826861,8.81220383694267));
#17304=CARTESIAN_POINT('Ctrl Pts',(-5.70469256863376,5.00379700216032,8.86498466304636));
#17305=CARTESIAN_POINT('Ctrl Pts',(-6.09208369431142,5.04762573267528,8.91803146859742));
#17306=CARTESIAN_POINT('Ctrl Pts',(-6.47056983558372,4.94639948026783,8.97134097339838));
#17307=CARTESIAN_POINT('Ctrl Pts',(-6.78746858719032,4.71274045756303,9.02490910160121));
#17308=CARTESIAN_POINT('Ctrl Pts',(-6.99804433390308,4.37791298839973,9.07873133117115));
#17309=CARTESIAN_POINT('Ctrl Pts',(-7.07219332762122,3.98740319786627,9.13280196225214));
#17310=CARTESIAN_POINT('Ctrl Pts',(-6.99796865015276,3.59525453990437,9.18711581050414));
#17311=CARTESIAN_POINT('Ctrl Pts',(-6.76140078434104,3.2176912418475,9.24772569638974));
#17312=CARTESIAN_POINT('Ctrl Pts',(-6.34225949707073,2.94654602106377,9.31472311482269));
#17313=CARTESIAN_POINT('Ctrl Pts',(-5.79639322685134,2.90560751314568,9.3882003670644));
#17314=CARTESIAN_POINT('Ctrl Pts',(-5.27370444272467,3.14075473304909,9.46511866155133));
#17315=CARTESIAN_POINT('Ctrl Pts',(-4.92371803536237,3.63287013680252,9.54550949397408));
#17316=CARTESIAN_POINT('Ctrl Pts',(-4.88802166561496,4.26218457037089,9.62939471067557));
#17317=CARTESIAN_POINT('Ctrl Pts',(-5.19387931501792,4.81633827697949,9.71364499530948));
#17318=CARTESIAN_POINT('Ctrl Pts',(-5.74991952335929,5.12402428928409,9.79822162675657));
#17319=CARTESIAN_POINT('Ctrl Pts',(-6.38656191712891,5.0885391306891,9.88308361150577));
#17320=CARTESIAN_POINT('Ctrl Pts',(-6.90822667172928,4.71869213404092,9.96818846822383));
#17321=CARTESIAN_POINT('Ctrl Pts',(-7.15369278117839,4.12658524801911,10.0534921977017));
#17322=CARTESIAN_POINT('Ctrl Pts',(-7.04627827661993,3.49350501160261,10.1389496543118));
#17323=CARTESIAN_POINT('Ctrl Pts',(-6.61793136444462,3.0140348706312,10.2245147901346));
#17324=CARTESIAN_POINT('Ctrl Pts',(-5.99969047434799,2.83587138114131,10.3101409223404));
#17325=CARTESIAN_POINT('Ctrl Pts',(-5.38133414015581,3.01401924516413,10.3957810076217));
#17326=CARTESIAN_POINT('Ctrl Pts',(-4.95274187669847,3.49369758179628,10.481387897791));
#17327=CARTESIAN_POINT('Ctrl Pts',(-4.84520028211577,4.12729592446544,10.5669146789137));
#17328=CARTESIAN_POINT('Ctrl Pts',(-5.09092458014618,4.72009886759013,10.6523148677484));
#17329=CARTESIAN_POINT('Ctrl Pts',(-5.61335583694406,5.09051867229157,10.7375427577537));
#17330=CARTESIAN_POINT('Ctrl Pts',(-6.25117077894511,5.12607085917612,10.8225535720965));
#17331=CARTESIAN_POINT('Ctrl Pts',(-6.80841662056156,4.81774324430063,10.9073040023736));
#17332=CARTESIAN_POINT('Ctrl Pts',(-7.11508736240155,4.2621592301609,10.9917518238937));
#17333=CARTESIAN_POINT('Ctrl Pts',(-7.0792883317528,3.63115822330435,11.0758574987941));
#17334=CARTESIAN_POINT('Ctrl Pts',(-6.71491091945052,3.11823669279566,11.1595814344114));
#17335=CARTESIAN_POINT('Ctrl Pts',(-6.13641410951145,2.87910001310329,11.2428908007876));
#17336=CARTESIAN_POINT('Ctrl Pts',(-5.52273543986151,2.98368129161145,11.3257449331281));
#17337=CARTESIAN_POINT('Ctrl Pts',(-5.06157565192072,3.39673596202277,11.4081288381091));
#17338=CARTESIAN_POINT('Ctrl Pts',(-4.94849818871645,3.79037870846202,11.4626969504328));
#17339=CARTESIAN_POINT('Ctrl Pts',(-4.94847164137573,3.98757933453,11.4899208404099));
#17340=CARTESIAN_POINT('Ctrl Pts',(-5.00000184100681,4.0136754734751,2.60093950625076));
#17341=CARTESIAN_POINT('Ctrl Pts',(-5.00002711936209,4.20144961727963,2.62686205390075));
#17342=CARTESIAN_POINT('Ctrl Pts',(-5.1076914443916,4.57620101292901,2.67882571929646));
#17343=CARTESIAN_POINT('Ctrl Pts',(-5.54731085839696,4.97011855968613,2.75738770095752));
#17344=CARTESIAN_POINT('Ctrl Pts',(-6.13330829028169,5.07009398433603,2.83651804650349));
#17345=CARTESIAN_POINT('Ctrl Pts',(-6.68676060294283,4.84148936906199,2.91622569034364));
#17346=CARTESIAN_POINT('Ctrl Pts',(-7.03617542740839,4.34995411926946,2.99649057036664));
#17347=CARTESIAN_POINT('Ctrl Pts',(-7.07077171566156,3.74380977688242,3.07730075350998));
#17348=CARTESIAN_POINT('Ctrl Pts',(-6.77566001133407,3.20870450421941,3.15863603264667));
#17349=CARTESIAN_POINT('Ctrl Pts',(-6.23777975703619,2.91082274760045,3.24047540010177));
#17350=CARTESIAN_POINT('Ctrl Pts',(-5.62027751939497,2.94499359194798,3.32279385402167));
#17351=CARTESIAN_POINT('Ctrl Pts',(-5.1128578559771,3.30444603110391,3.40556404882598));
#17352=CARTESIAN_POINT('Ctrl Pts',(-4.87328209631149,3.88170381609706,3.48875576249667));
#17353=CARTESIAN_POINT('Ctrl Pts',(-4.97806047014568,4.50081578134862,3.57233636795591));
#17354=CARTESIAN_POINT('Ctrl Pts',(-5.39799694068156,4.97124635132397,3.65627091939543));
#17355=CARTESIAN_POINT('Ctrl Pts',(-6.00608186722498,5.1467635917961,3.7405223892875));
#17356=CARTESIAN_POINT('Ctrl Pts',(-6.61648592829516,4.97125245378467,3.82505187703477));
#17357=CARTESIAN_POINT('Ctrl Pts',(-7.02504723026834,4.51407458863333,3.90667930466183));
#17358=CARTESIAN_POINT('Ctrl Pts',(-7.14109507248108,3.93953170138583,3.98533819578826));
#17359=CARTESIAN_POINT('Ctrl Pts',(-6.97515546374893,3.40104443225745,4.06097495793453));
#17360=CARTESIAN_POINT('Ctrl Pts',(-6.57122653386479,3.00706128325563,4.13670514732847));
#17361=CARTESIAN_POINT('Ctrl Pts',(-6.02775857632327,2.85377271371871,4.21249751130402));
#17362=CARTESIAN_POINT('Ctrl Pts',(-5.47693199324532,2.97976879840739,4.28832050275612));
#17363=CARTESIAN_POINT('Ctrl Pts',(-5.08889329636147,3.32248782371839,4.35782394322737));
#17364=CARTESIAN_POINT('Ctrl Pts',(-4.90348334427995,3.74815768282725,4.42098503121462));
#17365=CARTESIAN_POINT('Ctrl Pts',(-4.88777846541416,4.16541417756998,4.47779829335302));
#17366=CARTESIAN_POINT('Ctrl Pts',(-5.02572337488508,4.5591407782775,4.53456660974454));
#17367=CARTESIAN_POINT('Ctrl Pts',(-5.32762081329308,4.91046292297288,4.59757802398128));
#17368=CARTESIAN_POINT('Ctrl Pts',(-5.79769987729577,5.12240617534609,4.6667893141555));
#17369=CARTESIAN_POINT('Ctrl Pts',(-6.35744977854988,5.0800953582818,4.74213609062164));
#17370=CARTESIAN_POINT('Ctrl Pts',(-6.7886388886812,4.80135715932747,4.81103357029135));
#17371=CARTESIAN_POINT('Ctrl Pts',(-7.03217914396847,4.41239214657722,4.87351124701705));
#17372=CARTESIAN_POINT('Ctrl Pts',(-7.13592863330475,3.87207852021905,4.94830807653976));
#17373=CARTESIAN_POINT('Ctrl Pts',(-6.87284718079957,3.20107467373212,5.04144479366485));
#17374=CARTESIAN_POINT('Ctrl Pts',(-6.09623481157017,2.82823992504595,5.15254762809713));
#17375=CARTESIAN_POINT('Ctrl Pts',(-5.27971004197149,3.08146490109176,5.26291010705797));
#17376=CARTESIAN_POINT('Ctrl Pts',(-4.85635349881296,3.81715131471987,5.37246078991772));
#17377=CARTESIAN_POINT('Ctrl Pts',(-5.04487949063783,4.63769677411038,5.48113679376609));
#17378=CARTESIAN_POINT('Ctrl Pts',(-5.73589746055469,5.10693196272956,5.58888446285182));
#17379=CARTESIAN_POINT('Ctrl Pts',(-6.37118793757295,5.00949360744693,5.67193196549858));
#17380=CARTESIAN_POINT('Ctrl Pts',(-6.71254361053678,4.74926813559046,5.73087908447486));
#17381=CARTESIAN_POINT('Ctrl Pts',(-6.92618421314144,4.48213635150675,5.77788659686335));
#17382=CARTESIAN_POINT('Ctrl Pts',(-7.05447791083229,4.06557532936466,5.83636209009091));
#17383=CARTESIAN_POINT('Ctrl Pts',(-6.95088091422359,3.55670409484484,5.90607316301112));
#17384=CARTESIAN_POINT('Ctrl Pts',(-6.61900788359635,3.16160526086392,5.97532164754671));
#17385=CARTESIAN_POINT('Ctrl Pts',(-6.14183402203666,2.97493714351951,6.0441065734333));
#17386=CARTESIAN_POINT('Ctrl Pts',(-5.67880942079896,3.03347123408109,6.10673564359386));
#17387=CARTESIAN_POINT('Ctrl Pts',(-5.32735160410172,3.25520230218429,6.16333652454754));
#17388=CARTESIAN_POINT('Ctrl Pts',(-5.03108251682038,3.65479384285351,6.23091649770626));
#17389=CARTESIAN_POINT('Ctrl Pts',(-4.99209121035488,4.17131828916311,6.29799027327816));
#17390=CARTESIAN_POINT('Ctrl Pts',(-5.22308647377139,4.60388582873653,6.36457330678434));
#17391=CARTESIAN_POINT('Ctrl Pts',(-5.49945070307415,4.84205518395227,6.4142703184249));
#17392=CARTESIAN_POINT('Ctrl Pts',(-5.8429108649416,4.96183684549319,6.46373244635463));
#17393=CARTESIAN_POINT('Ctrl Pts',(-6.26484181971828,4.94625056066266,6.52117144061682));
#17394=CARTESIAN_POINT('Ctrl Pts',(-6.69390577408147,4.70907736638303,6.58644589945804));
#17395=CARTESIAN_POINT('Ctrl Pts',(-6.95873462103172,4.22881797506906,6.65940509116432));
#17396=CARTESIAN_POINT('Ctrl Pts',(-6.93269246532923,3.77588585116234,6.71983222414211));
#17397=CARTESIAN_POINT('Ctrl Pts',(-6.77107468324783,3.46412923688142,6.7679659145118));
#17398=CARTESIAN_POINT('Ctrl Pts',(-6.57079871082626,3.25210408080074,6.80796630929164));
#17399=CARTESIAN_POINT('Ctrl Pts',(-6.28566327773964,3.10148204150563,6.85183024182226));
#17400=CARTESIAN_POINT('Ctrl Pts',(-5.9374350403567,3.06238692304077,6.89952195896654));
#17401=CARTESIAN_POINT('Ctrl Pts',(-5.54350254185785,3.16770824417749,6.95498839067594));
#17402=CARTESIAN_POINT('Ctrl Pts',(-5.18977130243312,3.48372162057587,7.01814871426604));
#17403=CARTESIAN_POINT('Ctrl Pts',(-5.04285761799324,3.99497433346206,7.0889328817521));
#17404=CARTESIAN_POINT('Ctrl Pts',(-5.18978309684873,4.50416337482064,7.15948666242575));
#17405=CARTESIAN_POINT('Ctrl Pts',(-5.58408091231752,4.85632154197909,7.22985222665258));
#17406=CARTESIAN_POINT('Ctrl Pts',(-6.10418851591415,4.94454356395432,7.30007283487924));
#17407=CARTESIAN_POINT('Ctrl Pts',(-6.59084588507658,4.74288104801731,7.37019262264957));
#17408=CARTESIAN_POINT('Ctrl Pts',(-6.89540829263521,4.31357351131412,7.44025632549589));
#17409=CARTESIAN_POINT('Ctrl Pts',(-6.92492923689232,3.78812028153619,7.51030900574892));
#17410=CARTESIAN_POINT('Ctrl Pts',(-6.67028427013333,3.32725098620657,7.58039577698737));
#17411=CARTESIAN_POINT('Ctrl Pts',(-6.20897623341015,3.0721729365591,7.65056157443552));
#17412=CARTESIAN_POINT('Ctrl Pts',(-5.68173783558839,3.10162769981329,7.72085085716389));
#17413=CARTESIAN_POINT('Ctrl Pts',(-5.24992919279951,3.40776503869049,7.79130734597953));
#17414=CARTESIAN_POINT('Ctrl Pts',(-5.0465424843122,3.89815513625059,7.86197377424775));
#17415=CARTESIAN_POINT('Ctrl Pts',(-5.13549244911485,4.42345796985394,7.9328916443029));
#17416=CARTESIAN_POINT('Ctrl Pts',(-5.49174629490197,4.82258141736487,8.00410096577713));
#17417=CARTESIAN_POINT('Ctrl Pts',(-6.00803868168598,4.97171279548103,8.07564000534741));
#17418=CARTESIAN_POINT('Ctrl Pts',(-6.52735154266829,4.82257974695955,8.1475451059773));
#17419=CARTESIAN_POINT('Ctrl Pts',(-6.87597910605558,4.43277936154282,8.2171724616343));
#17420=CARTESIAN_POINT('Ctrl Pts',(-6.97565473561711,3.94102818366579,8.28449961898768));
#17421=CARTESIAN_POINT('Ctrl Pts',(-6.8330580514463,3.47827883486752,8.34949563910535));
#17422=CARTESIAN_POINT('Ctrl Pts',(-6.51380412257741,3.1662390255362,8.40942447363317));
#17423=CARTESIAN_POINT('Ctrl Pts',(-6.13368043091516,3.03340218960474,8.46419547601407));
#17424=CARTESIAN_POINT('Ctrl Pts',(-5.77000963425156,3.04672415558585,8.51371979129401));
#17425=CARTESIAN_POINT('Ctrl Pts',(-5.43474033823938,3.19292650787483,8.56348049163152));
#17426=CARTESIAN_POINT('Ctrl Pts',(-5.17477216956946,3.45264130135924,8.61348288970698));
#17427=CARTESIAN_POINT('Ctrl Pts',(-5.02692180394174,3.79107624660051,8.6637316830418));
#17428=CARTESIAN_POINT('Ctrl Pts',(-5.012872576251,4.16195256384123,8.7142309145088));
#17429=CARTESIAN_POINT('Ctrl Pts',(-5.13590369868626,4.51409239039593,8.76498396821864));
#17430=CARTESIAN_POINT('Ctrl Pts',(-5.38031427946466,4.79836661872066,8.81599356007185));
#17431=CARTESIAN_POINT('Ctrl Pts',(-5.71336668770006,4.97458793379134,8.86726173279411));
#17432=CARTESIAN_POINT('Ctrl Pts',(-6.08968356313292,5.01715924274108,8.918789847283));
#17433=CARTESIAN_POINT('Ctrl Pts',(-6.45738481100365,4.91881570416212,8.9705785818587));
#17434=CARTESIAN_POINT('Ctrl Pts',(-6.76530671813857,4.69177684003305,9.02262792715958));
#17435=CARTESIAN_POINT('Ctrl Pts',(-6.96997065785482,4.36635789720065,9.07493719271063));
#17436=CARTESIAN_POINT('Ctrl Pts',(-7.04206467317586,3.98670152421777,9.12750499448518));
#17437=CARTESIAN_POINT('Ctrl Pts',(-6.96988775131722,3.60530323601265,9.18032928987629));
#17438=CARTESIAN_POINT('Ctrl Pts',(-6.7397150976367,3.23792225540337,9.23930487839808));
#17439=CARTESIAN_POINT('Ctrl Pts',(-6.33166237507248,2.97390330552954,9.30453505300732));
#17440=CARTESIAN_POINT('Ctrl Pts',(-5.79979171434613,2.93396143628525,9.37613052323128));
#17441=CARTESIAN_POINT('Ctrl Pts',(-5.29001663621426,3.16323503239153,9.45115011122364));
#17442=CARTESIAN_POINT('Ctrl Pts',(-4.94825545210904,3.64363042187255,9.52964181259955));
#17443=CARTESIAN_POINT('Ctrl Pts',(-4.91325516498484,4.25878443889604,9.61164803507556));
#17444=CARTESIAN_POINT('Ctrl Pts',(-5.2125378502354,4.80126773521892,9.69412424268727));
#17445=CARTESIAN_POINT('Ctrl Pts',(-5.75754644935023,5.10299443985526,9.77704205666351));
#17446=CARTESIAN_POINT('Ctrl Pts',(-6.38261067907029,5.06829058753974,9.86037045595682));
#17447=CARTESIAN_POINT('Ctrl Pts',(-6.89571009340608,4.70469230712254,9.94407602284259));
#17448=CARTESIAN_POINT('Ctrl Pts',(-7.13766387710299,4.12145232028498,10.0281230888647));
#17449=CARTESIAN_POINT('Ctrl Pts',(-7.03181245317105,3.49664097659948,10.112473958668));
#17450=CARTESIAN_POINT('Ctrl Pts',(-6.60841264630813,3.02246212675956,10.1970891533592));
#17451=CARTESIAN_POINT('Ctrl Pts',(-5.99601006835875,2.8458044826624,10.2819276244449));
#17452=CARTESIAN_POINT('Ctrl Pts',(-5.38219522105592,3.02246199100347,10.3669470032346));
#17453=CARTESIAN_POINT('Ctrl Pts',(-4.95579995827654,3.49941222674329,10.452103831618));
#17454=CARTESIAN_POINT('Ctrl Pts',(-4.84844583817861,4.13081136700949,10.5373538681711));
#17455=CARTESIAN_POINT('Ctrl Pts',(-5.0936581339001,4.72286468788687,10.6226522983686));
#17456=CARTESIAN_POINT('Ctrl Pts',(-5.61632959368519,5.09368411438882,10.7079540155997));
#17457=CARTESIAN_POINT('Ctrl Pts',(-6.25587144748665,5.12951914158568,10.7932138961696));
#17458=CARTESIAN_POINT('Ctrl Pts',(-6.81586867421465,4.81987787722662,10.8783870694892));
#17459=CARTESIAN_POINT('Ctrl Pts',(-7.12478685219004,4.26058878480156,10.9634291596385));
#17460=CARTESIAN_POINT('Ctrl Pts',(-7.08884111245123,3.62399110135786,11.0482965343607));
#17461=CARTESIAN_POINT('Ctrl Pts',(-6.72064073263906,3.10540887765364,11.132946666915));
#17462=CARTESIAN_POINT('Ctrl Pts',(-6.13478909423228,2.86304904084892,11.2173381176655));
#17463=CARTESIAN_POINT('Ctrl Pts',(-5.51202996456676,2.96902046658306,11.3014313460436));
#17464=CARTESIAN_POINT('Ctrl Pts',(-5.04310782052529,3.38875866553956,11.3851878225675));
#17465=CARTESIAN_POINT('Ctrl Pts',(-4.92780437314741,3.78964966219835,11.4407823887586));
#17466=CARTESIAN_POINT('Ctrl Pts',(-4.9277773302074,3.99053173009658,11.468514508194));
#17467=CARTESIAN_POINT('',(-5.00000184100681,4.0136754734751,2.60093950625076));
#17468=CARTESIAN_POINT('Origin',(-5.,4.,2.7));
#17469=CARTESIAN_POINT('',(-4.9277773302074,3.99053173009658,11.468514508194));
#17470=CARTESIAN_POINT('Ctrl Pts',(-5.00000184100681,4.0136754734751,2.60093950625076));
#17471=CARTESIAN_POINT('Ctrl Pts',(-5.00002711936209,4.20144961727963,2.62686205390075));
#17472=CARTESIAN_POINT('Ctrl Pts',(-5.1076914443916,4.57620101292901,2.67882571929646));
#17473=CARTESIAN_POINT('Ctrl Pts',(-5.54731085839696,4.97011855968613,2.75738770095752));
#17474=CARTESIAN_POINT('Ctrl Pts',(-6.13330829028169,5.07009398433603,2.83651804650349));
#17475=CARTESIAN_POINT('Ctrl Pts',(-6.68676060294283,4.84148936906199,2.91622569034364));
#17476=CARTESIAN_POINT('Ctrl Pts',(-7.03617542740839,4.34995411926946,2.99649057036664));
#17477=CARTESIAN_POINT('Ctrl Pts',(-7.07077171566156,3.74380977688242,3.07730075350998));
#17478=CARTESIAN_POINT('Ctrl Pts',(-6.77566001133407,3.20870450421941,3.15863603264667));
#17479=CARTESIAN_POINT('Ctrl Pts',(-6.23777975703619,2.91082274760045,3.24047540010177));
#17480=CARTESIAN_POINT('Ctrl Pts',(-5.62027751939497,2.94499359194798,3.32279385402167));
#17481=CARTESIAN_POINT('Ctrl Pts',(-5.1128578559771,3.30444603110391,3.40556404882598));
#17482=CARTESIAN_POINT('Ctrl Pts',(-4.87328209631149,3.88170381609706,3.48875576249667));
#17483=CARTESIAN_POINT('Ctrl Pts',(-4.97806047014568,4.50081578134862,3.57233636795591));
#17484=CARTESIAN_POINT('Ctrl Pts',(-5.39799694068156,4.97124635132397,3.65627091939543));
#17485=CARTESIAN_POINT('Ctrl Pts',(-6.00608186722498,5.1467635917961,3.7405223892875));
#17486=CARTESIAN_POINT('Ctrl Pts',(-6.61648592829516,4.97125245378467,3.82505187703477));
#17487=CARTESIAN_POINT('Ctrl Pts',(-7.02504723026834,4.51407458863333,3.90667930466183));
#17488=CARTESIAN_POINT('Ctrl Pts',(-7.14109507248108,3.93953170138583,3.98533819578826));
#17489=CARTESIAN_POINT('Ctrl Pts',(-6.97515546374893,3.40104443225745,4.06097495793453));
#17490=CARTESIAN_POINT('Ctrl Pts',(-6.57122653386479,3.00706128325563,4.13670514732847));
#17491=CARTESIAN_POINT('Ctrl Pts',(-6.02775857632327,2.85377271371871,4.21249751130402));
#17492=CARTESIAN_POINT('Ctrl Pts',(-5.47693199324532,2.97976879840739,4.28832050275612));
#17493=CARTESIAN_POINT('Ctrl Pts',(-5.08889329636147,3.32248782371839,4.35782394322737));
#17494=CARTESIAN_POINT('Ctrl Pts',(-4.90348334427995,3.74815768282725,4.42098503121462));
#17495=CARTESIAN_POINT('Ctrl Pts',(-4.88777846541416,4.16541417756998,4.47779829335302));
#17496=CARTESIAN_POINT('Ctrl Pts',(-5.02572337488508,4.5591407782775,4.53456660974454));
#17497=CARTESIAN_POINT('Ctrl Pts',(-5.32762081329308,4.91046292297288,4.59757802398128));
#17498=CARTESIAN_POINT('Ctrl Pts',(-5.79769987729577,5.12240617534609,4.6667893141555));
#17499=CARTESIAN_POINT('Ctrl Pts',(-6.35744977854988,5.0800953582818,4.74213609062164));
#17500=CARTESIAN_POINT('Ctrl Pts',(-6.7886388886812,4.80135715932747,4.81103357029135));
#17501=CARTESIAN_POINT('Ctrl Pts',(-7.03217914396847,4.41239214657722,4.87351124701705));
#17502=CARTESIAN_POINT('Ctrl Pts',(-7.13592863330475,3.87207852021905,4.94830807653976));
#17503=CARTESIAN_POINT('Ctrl Pts',(-6.87284718079957,3.20107467373212,5.04144479366485));
#17504=CARTESIAN_POINT('Ctrl Pts',(-6.09623481157017,2.82823992504595,5.15254762809713));
#17505=CARTESIAN_POINT('Ctrl Pts',(-5.27971004197149,3.08146490109176,5.26291010705797));
#17506=CARTESIAN_POINT('Ctrl Pts',(-4.85635349881296,3.81715131471987,5.37246078991772));
#17507=CARTESIAN_POINT('Ctrl Pts',(-5.04487949063783,4.63769677411038,5.48113679376609));
#17508=CARTESIAN_POINT('Ctrl Pts',(-5.73589746055469,5.10693196272956,5.58888446285182));
#17509=CARTESIAN_POINT('Ctrl Pts',(-6.37118793757295,5.00949360744693,5.67193196549858));
#17510=CARTESIAN_POINT('Ctrl Pts',(-6.71254361053678,4.74926813559046,5.73087908447486));
#17511=CARTESIAN_POINT('Ctrl Pts',(-6.92618421314144,4.48213635150675,5.77788659686335));
#17512=CARTESIAN_POINT('Ctrl Pts',(-7.05447791083229,4.06557532936466,5.83636209009091));
#17513=CARTESIAN_POINT('Ctrl Pts',(-6.95088091422359,3.55670409484484,5.90607316301112));
#17514=CARTESIAN_POINT('Ctrl Pts',(-6.61900788359635,3.16160526086392,5.97532164754671));
#17515=CARTESIAN_POINT('Ctrl Pts',(-6.14183402203666,2.97493714351951,6.0441065734333));
#17516=CARTESIAN_POINT('Ctrl Pts',(-5.67880942079896,3.03347123408109,6.10673564359386));
#17517=CARTESIAN_POINT('Ctrl Pts',(-5.32735160410172,3.25520230218429,6.16333652454754));
#17518=CARTESIAN_POINT('Ctrl Pts',(-5.03108251682038,3.65479384285351,6.23091649770626));
#17519=CARTESIAN_POINT('Ctrl Pts',(-4.99209121035488,4.17131828916311,6.29799027327816));
#17520=CARTESIAN_POINT('Ctrl Pts',(-5.22308647377139,4.60388582873653,6.36457330678434));
#17521=CARTESIAN_POINT('Ctrl Pts',(-5.49945070307415,4.84205518395227,6.4142703184249));
#17522=CARTESIAN_POINT('Ctrl Pts',(-5.8429108649416,4.96183684549319,6.46373244635463));
#17523=CARTESIAN_POINT('Ctrl Pts',(-6.26484181971828,4.94625056066266,6.52117144061682));
#17524=CARTESIAN_POINT('Ctrl Pts',(-6.69390577408147,4.70907736638303,6.58644589945804));
#17525=CARTESIAN_POINT('Ctrl Pts',(-6.95873462103172,4.22881797506906,6.65940509116432));
#17526=CARTESIAN_POINT('Ctrl Pts',(-6.93269246532923,3.77588585116234,6.71983222414211));
#17527=CARTESIAN_POINT('Ctrl Pts',(-6.77107468324783,3.46412923688142,6.7679659145118));
#17528=CARTESIAN_POINT('Ctrl Pts',(-6.57079871082626,3.25210408080074,6.80796630929164));
#17529=CARTESIAN_POINT('Ctrl Pts',(-6.28566327773964,3.10148204150563,6.85183024182226));
#17530=CARTESIAN_POINT('Ctrl Pts',(-5.9374350403567,3.06238692304077,6.89952195896654));
#17531=CARTESIAN_POINT('Ctrl Pts',(-5.54350254185785,3.16770824417749,6.95498839067594));
#17532=CARTESIAN_POINT('Ctrl Pts',(-5.18977130243312,3.48372162057587,7.01814871426604));
#17533=CARTESIAN_POINT('Ctrl Pts',(-5.04285761799324,3.99497433346206,7.0889328817521));
#17534=CARTESIAN_POINT('Ctrl Pts',(-5.18978309684873,4.50416337482064,7.15948666242575));
#17535=CARTESIAN_POINT('Ctrl Pts',(-5.58408091231752,4.85632154197909,7.22985222665258));
#17536=CARTESIAN_POINT('Ctrl Pts',(-6.10418851591415,4.94454356395432,7.30007283487924));
#17537=CARTESIAN_POINT('Ctrl Pts',(-6.59084588507658,4.74288104801731,7.37019262264957));
#17538=CARTESIAN_POINT('Ctrl Pts',(-6.89540829263521,4.31357351131412,7.44025632549589));
#17539=CARTESIAN_POINT('Ctrl Pts',(-6.92492923689232,3.78812028153619,7.51030900574892));
#17540=CARTESIAN_POINT('Ctrl Pts',(-6.67028427013333,3.32725098620657,7.58039577698737));
#17541=CARTESIAN_POINT('Ctrl Pts',(-6.20897623341015,3.0721729365591,7.65056157443552));
#17542=CARTESIAN_POINT('Ctrl Pts',(-5.68173783558839,3.10162769981329,7.72085085716389));
#17543=CARTESIAN_POINT('Ctrl Pts',(-5.24992919279951,3.40776503869049,7.79130734597953));
#17544=CARTESIAN_POINT('Ctrl Pts',(-5.0465424843122,3.89815513625059,7.86197377424775));
#17545=CARTESIAN_POINT('Ctrl Pts',(-5.13549244911485,4.42345796985394,7.9328916443029));
#17546=CARTESIAN_POINT('Ctrl Pts',(-5.49174629490197,4.82258141736487,8.00410096577713));
#17547=CARTESIAN_POINT('Ctrl Pts',(-6.00803868168598,4.97171279548103,8.07564000534741));
#17548=CARTESIAN_POINT('Ctrl Pts',(-6.52735154266829,4.82257974695955,8.1475451059773));
#17549=CARTESIAN_POINT('Ctrl Pts',(-6.87597910605558,4.43277936154282,8.2171724616343));
#17550=CARTESIAN_POINT('Ctrl Pts',(-6.97565473561711,3.94102818366579,8.28449961898768));
#17551=CARTESIAN_POINT('Ctrl Pts',(-6.8330580514463,3.47827883486752,8.34949563910535));
#17552=CARTESIAN_POINT('Ctrl Pts',(-6.51380412257741,3.1662390255362,8.40942447363317));
#17553=CARTESIAN_POINT('Ctrl Pts',(-6.13368043091516,3.03340218960474,8.46419547601407));
#17554=CARTESIAN_POINT('Ctrl Pts',(-5.77000963425156,3.04672415558585,8.51371979129401));
#17555=CARTESIAN_POINT('Ctrl Pts',(-5.43474033823938,3.19292650787483,8.56348049163152));
#17556=CARTESIAN_POINT('Ctrl Pts',(-5.17477216956946,3.45264130135924,8.61348288970698));
#17557=CARTESIAN_POINT('Ctrl Pts',(-5.02692180394174,3.79107624660051,8.6637316830418));
#17558=CARTESIAN_POINT('Ctrl Pts',(-5.012872576251,4.16195256384123,8.7142309145088));
#17559=CARTESIAN_POINT('Ctrl Pts',(-5.13590369868626,4.51409239039593,8.76498396821864));
#17560=CARTESIAN_POINT('Ctrl Pts',(-5.38031427946466,4.79836661872066,8.81599356007185));
#17561=CARTESIAN_POINT('Ctrl Pts',(-5.71336668770006,4.97458793379134,8.86726173279411));
#17562=CARTESIAN_POINT('Ctrl Pts',(-6.08968356313292,5.01715924274108,8.918789847283));
#17563=CARTESIAN_POINT('Ctrl Pts',(-6.45738481100365,4.91881570416212,8.9705785818587));
#17564=CARTESIAN_POINT('Ctrl Pts',(-6.76530671813857,4.69177684003305,9.02262792715958));
#17565=CARTESIAN_POINT('Ctrl Pts',(-6.96997065785482,4.36635789720065,9.07493719271063));
#17566=CARTESIAN_POINT('Ctrl Pts',(-7.04206467317586,3.98670152421777,9.12750499448518));
#17567=CARTESIAN_POINT('Ctrl Pts',(-6.96988775131722,3.60530323601265,9.18032928987629));
#17568=CARTESIAN_POINT('Ctrl Pts',(-6.7397150976367,3.23792225540337,9.23930487839808));
#17569=CARTESIAN_POINT('Ctrl Pts',(-6.33166237507248,2.97390330552954,9.30453505300732));
#17570=CARTESIAN_POINT('Ctrl Pts',(-5.79979171434613,2.93396143628525,9.37613052323128));
#17571=CARTESIAN_POINT('Ctrl Pts',(-5.29001663621426,3.16323503239153,9.45115011122364));
#17572=CARTESIAN_POINT('Ctrl Pts',(-4.94825545210904,3.64363042187255,9.52964181259955));
#17573=CARTESIAN_POINT('Ctrl Pts',(-4.91325516498484,4.25878443889604,9.61164803507556));
#17574=CARTESIAN_POINT('Ctrl Pts',(-5.2125378502354,4.80126773521892,9.69412424268727));
#17575=CARTESIAN_POINT('Ctrl Pts',(-5.75754644935023,5.10299443985526,9.77704205666351));
#17576=CARTESIAN_POINT('Ctrl Pts',(-6.38261067907029,5.06829058753974,9.86037045595682));
#17577=CARTESIAN_POINT('Ctrl Pts',(-6.89571009340608,4.70469230712254,9.94407602284259));
#17578=CARTESIAN_POINT('Ctrl Pts',(-7.13766387710299,4.12145232028498,10.0281230888647));
#17579=CARTESIAN_POINT('Ctrl Pts',(-7.03181245317105,3.49664097659948,10.112473958668));
#17580=CARTESIAN_POINT('Ctrl Pts',(-6.60841264630813,3.02246212675956,10.1970891533592));
#17581=CARTESIAN_POINT('Ctrl Pts',(-5.99601006835875,2.8458044826624,10.2819276244449));
#17582=CARTESIAN_POINT('Ctrl Pts',(-5.38219522105592,3.02246199100347,10.3669470032346));
#17583=CARTESIAN_POINT('Ctrl Pts',(-4.95579995827654,3.49941222674329,10.452103831618));
#17584=CARTESIAN_POINT('Ctrl Pts',(-4.84844583817861,4.13081136700949,10.5373538681711));
#17585=CARTESIAN_POINT('Ctrl Pts',(-5.0936581339001,4.72286468788687,10.6226522983686));
#17586=CARTESIAN_POINT('Ctrl Pts',(-5.61632959368519,5.09368411438882,10.7079540155997));
#17587=CARTESIAN_POINT('Ctrl Pts',(-6.25587144748665,5.12951914158568,10.7932138961696));
#17588=CARTESIAN_POINT('Ctrl Pts',(-6.81586867421465,4.81987787722662,10.8783870694892));
#17589=CARTESIAN_POINT('Ctrl Pts',(-7.12478685219004,4.26058878480156,10.9634291596385));
#17590=CARTESIAN_POINT('Ctrl Pts',(-7.08884111245123,3.62399110135786,11.0482965343607));
#17591=CARTESIAN_POINT('Ctrl Pts',(-6.72064073263906,3.10540887765364,11.132946666915));
#17592=CARTESIAN_POINT('Ctrl Pts',(-6.13478909423228,2.86304904084892,11.2173381176655));
#17593=CARTESIAN_POINT('Ctrl Pts',(-5.51202996456676,2.96902046658306,11.3014313460436));
#17594=CARTESIAN_POINT('Ctrl Pts',(-5.04310782052529,3.38875866553956,11.3851878225675));
#17595=CARTESIAN_POINT('Ctrl Pts',(-4.92780437314741,3.78964966219835,11.4407823887586));
#17596=CARTESIAN_POINT('Ctrl Pts',(-4.9277773302074,3.99053173009658,11.468514508194));
#17597=CARTESIAN_POINT('Origin',(-5.,4.,11.4));
#17598=CARTESIAN_POINT('Origin',(-5.,4.,11.4));
#17599=CARTESIAN_POINT('Origin',(-5.,4.,2.7));
#17600=CARTESIAN_POINT('',(0.,0.,0.));
#17601=CARTESIAN_POINT('Origin',(4.4,-1.3,-0.1));
#17602=CARTESIAN_POINT('',(4.19,-1.3,0.));
#17603=CARTESIAN_POINT('Origin',(4.4,-1.3,0.));
#17604=CARTESIAN_POINT('',(4.19,-1.3,0.9));
#17605=CARTESIAN_POINT('',(4.19,-1.3,-0.1));
#17606=CARTESIAN_POINT('Origin',(4.4,-1.3,0.9));
#17607=CARTESIAN_POINT('Origin',(4.4,-1.3,0.9));
#17608=CARTESIAN_POINT('Origin',(7.6,-1.3,-0.1));
#17609=CARTESIAN_POINT('',(7.39,-1.3,0.));
#17610=CARTESIAN_POINT('Origin',(7.6,-1.3,0.));
#17611=CARTESIAN_POINT('',(7.39,-1.3,0.9));
#17612=CARTESIAN_POINT('',(7.39,-1.3,-0.1));
#17613=CARTESIAN_POINT('Origin',(7.6,-1.3,0.9));
#17614=CARTESIAN_POINT('Origin',(7.6,-1.3,0.9));
#17615=CARTESIAN_POINT('Origin',(4.4,-1.8,1.2));
#17616=CARTESIAN_POINT('',(4.19,-1.7,1.2));
#17617=CARTESIAN_POINT('Origin',(4.4,-1.7,1.2));
#17618=CARTESIAN_POINT('',(4.19,-0.9,1.2));
#17619=CARTESIAN_POINT('',(4.19,-1.8,1.2));
#17620=CARTESIAN_POINT('Origin',(4.4,-0.9,1.2));
#17621=CARTESIAN_POINT('Origin',(7.6,-1.8,1.2));
#17622=CARTESIAN_POINT('',(7.39,-1.7,1.2));
#17623=CARTESIAN_POINT('Origin',(7.6,-1.7,1.2));
#17624=CARTESIAN_POINT('',(7.39,-0.9,1.2));
#17625=CARTESIAN_POINT('',(7.39,-1.8,1.2));
#17626=CARTESIAN_POINT('Origin',(7.6,-0.9,1.2));
#17627=CARTESIAN_POINT('Origin',(8.4,-0.9,0.));
#17628=CARTESIAN_POINT('',(8.4,-0.9,0.));
#17629=CARTESIAN_POINT('',(3.6,-0.9,0.));
#17630=CARTESIAN_POINT('',(8.4,-0.9,0.));
#17631=CARTESIAN_POINT('',(3.6,-0.9,3.));
#17632=CARTESIAN_POINT('',(3.6,-0.9,0.));
#17633=CARTESIAN_POINT('',(8.4,-0.9,3.));
#17634=CARTESIAN_POINT('',(8.4,-0.9,3.));
#17635=CARTESIAN_POINT('',(8.4,-0.9,0.));
#17636=CARTESIAN_POINT('Origin',(8.4,-1.7,0.));
#17637=CARTESIAN_POINT('',(8.4,-1.7,0.));
#17638=CARTESIAN_POINT('',(8.4,-1.7,0.));
#17639=CARTESIAN_POINT('',(8.4,-1.7,3.));
#17640=CARTESIAN_POINT('',(8.4,-1.7,3.));
#17641=CARTESIAN_POINT('',(8.4,-1.7,0.));
#17642=CARTESIAN_POINT('Origin',(3.6,-1.7,0.));
#17643=CARTESIAN_POINT('',(3.6,-1.7,0.));
#17644=CARTESIAN_POINT('',(3.6,-1.7,0.));
#17645=CARTESIAN_POINT('',(3.6,-1.7,3.));
#17646=CARTESIAN_POINT('',(3.6,-1.7,3.));
#17647=CARTESIAN_POINT('',(3.6,-1.7,0.));
#17648=CARTESIAN_POINT('Origin',(3.6,-0.9,0.));
#17649=CARTESIAN_POINT('',(3.6,-0.9,0.));
#17650=CARTESIAN_POINT('',(3.6,-0.9,3.));
#17651=CARTESIAN_POINT('Origin',(6.,-1.3,3.));
#17652=CARTESIAN_POINT('Origin',(6.,-1.3,0.));
#17653=CARTESIAN_POINT('',(0.,0.,0.));
#17654=CARTESIAN_POINT('Origin',(4.4,0.,29.6));
#17655=CARTESIAN_POINT('',(4.19,-2.57175827820944E-17,29.7));
#17656=CARTESIAN_POINT('Origin',(4.4,0.,29.7));
#17657=CARTESIAN_POINT('',(4.19,2.57175827820944E-17,30.5));
#17658=CARTESIAN_POINT('',(4.19,-2.57175827820944E-17,29.6));
#17659=CARTESIAN_POINT('Origin',(4.4,0.,30.5));
#17660=CARTESIAN_POINT('Origin',(7.6,0.,29.6));
#17661=CARTESIAN_POINT('',(7.39,-2.57175827820944E-17,29.7));
#17662=CARTESIAN_POINT('Origin',(7.6,0.,29.7));
#17663=CARTESIAN_POINT('',(7.39,2.57175827820944E-17,30.5));
#17664=CARTESIAN_POINT('',(7.39,-2.57175827820944E-17,29.6));
#17665=CARTESIAN_POINT('Origin',(7.6,0.,30.5));
#17666=CARTESIAN_POINT('Origin',(4.4,-1.8,29.8));
#17667=CARTESIAN_POINT('',(4.19,-1.7,29.8));
#17668=CARTESIAN_POINT('Origin',(4.4,-1.7,29.8));
#17669=CARTESIAN_POINT('',(4.19,-0.8,29.8));
#17670=CARTESIAN_POINT('',(4.19,-1.8,29.8));
#17671=CARTESIAN_POINT('',(4.58466185312619,-0.8,29.7));
#17672=CARTESIAN_POINT('Origin',(4.4,-0.8,29.8));
#17673=CARTESIAN_POINT('',(4.5846618531262,-0.9,29.7));
#17674=CARTESIAN_POINT('',(4.58466185312619,-1.8,29.7));
#17675=CARTESIAN_POINT('',(4.21533814687381,-0.9,29.7));
#17676=CARTESIAN_POINT('Origin',(4.4,-0.9,29.8));
#17677=CARTESIAN_POINT('',(4.21533814687381,-0.8,29.7));
#17678=CARTESIAN_POINT('',(4.21533814687381,-1.8,29.7));
#17679=CARTESIAN_POINT('Origin',(4.4,-0.8,29.8));
#17680=CARTESIAN_POINT('Origin',(4.4,-0.8,29.8));
#17681=CARTESIAN_POINT('',(6.4,-0.8,29.7));
#17682=CARTESIAN_POINT('Origin',(7.6,-1.8,29.8));
#17683=CARTESIAN_POINT('',(7.39,-1.7,29.8));
#17684=CARTESIAN_POINT('Origin',(7.6,-1.7,29.8));
#17685=CARTESIAN_POINT('',(7.39,-0.8,29.8));
#17686=CARTESIAN_POINT('',(7.39,-1.8,29.8));
#17687=CARTESIAN_POINT('',(7.78466185312619,-0.8,29.7));
#17688=CARTESIAN_POINT('Origin',(7.6,-0.8,29.8));
#17689=CARTESIAN_POINT('',(7.78466185312619,-0.9,29.7));
#17690=CARTESIAN_POINT('',(7.78466185312619,-1.8,29.7));
#17691=CARTESIAN_POINT('',(7.4153381468738,-0.9,29.7));
#17692=CARTESIAN_POINT('Origin',(7.6,-0.9,29.8));
#17693=CARTESIAN_POINT('',(7.41533814687381,-0.8,29.7));
#17694=CARTESIAN_POINT('',(7.41533814687381,-1.8,29.7));
#17695=CARTESIAN_POINT('Origin',(7.6,-0.8,29.8));
#17696=CARTESIAN_POINT('Origin',(7.6,-0.8,29.8));
#17697=CARTESIAN_POINT('',(8.,-0.8,29.7));
#17698=CARTESIAN_POINT('Origin',(8.4,-0.9,28.));
#17699=CARTESIAN_POINT('',(8.4,-0.9,29.7));
#17700=CARTESIAN_POINT('',(8.4,-0.9,29.7));
#17701=CARTESIAN_POINT('',(8.4,-0.9,29.7));
#17702=CARTESIAN_POINT('',(8.4,-0.9,28.));
#17703=CARTESIAN_POINT('',(8.4,-0.9,28.));
#17704=CARTESIAN_POINT('',(3.6,-0.9,28.));
#17705=CARTESIAN_POINT('',(8.4,-0.9,28.));
#17706=CARTESIAN_POINT('',(3.6,-0.9,29.7));
#17707=CARTESIAN_POINT('',(3.6,-0.9,28.));
#17708=CARTESIAN_POINT('',(8.4,-0.9,29.7));
#17709=CARTESIAN_POINT('Origin',(8.4,-1.7,29.7));
#17710=CARTESIAN_POINT('',(3.6,1.,29.7));
#17711=CARTESIAN_POINT('',(3.6,-1.7,29.7));
#17712=CARTESIAN_POINT('',(8.4,1.,29.7));
#17713=CARTESIAN_POINT('',(3.6,1.,29.7));
#17714=CARTESIAN_POINT('',(8.4,-1.7,29.7));
#17715=CARTESIAN_POINT('Origin',(6.,1.,30.1));
#17716=CARTESIAN_POINT('',(3.6,1.,30.5));
#17717=CARTESIAN_POINT('',(8.4,1.,30.5));
#17718=CARTESIAN_POINT('',(8.4,1.,30.5));
#17719=CARTESIAN_POINT('',(8.4,1.,29.7));
#17720=CARTESIAN_POINT('',(3.6,1.,30.5));
#17721=CARTESIAN_POINT('Origin',(8.4,-1.7,28.));
#17722=CARTESIAN_POINT('',(8.4,-1.7,28.));
#17723=CARTESIAN_POINT('',(8.4,-1.7,30.5));
#17724=CARTESIAN_POINT('',(8.4,-1.7,28.));
#17725=CARTESIAN_POINT('',(8.4,-1.7,28.));
#17726=CARTESIAN_POINT('',(8.4,-1.7,30.5));
#17727=CARTESIAN_POINT('Origin',(3.6,-1.7,28.));
#17728=CARTESIAN_POINT('',(3.6,-1.7,28.));
#17729=CARTESIAN_POINT('',(3.6,-1.7,30.5));
#17730=CARTESIAN_POINT('',(3.6,-1.7,28.));
#17731=CARTESIAN_POINT('',(3.6,-1.7,28.));
#17732=CARTESIAN_POINT('',(3.6,-1.7,30.5));
#17733=CARTESIAN_POINT('Origin',(3.6,-0.9,28.));
#17734=CARTESIAN_POINT('',(3.6,-0.9,28.));
#17735=CARTESIAN_POINT('',(3.6,-1.7,30.5));
#17736=CARTESIAN_POINT('Origin',(6.,-1.3,30.5));
#17737=CARTESIAN_POINT('Origin',(6.,-1.3,28.));
#17738=CARTESIAN_POINT('',(0.,0.,0.));
#17739=CARTESIAN_POINT('Origin',(6.,-4.,1.9));
#17740=CARTESIAN_POINT('',(5.375,-4.,2.6));
#17741=CARTESIAN_POINT('Origin',(6.,-4.,2.6));
#17742=CARTESIAN_POINT('',(5.375,-4.,1.9));
#17743=CARTESIAN_POINT('',(5.375,-4.,1.9));
#17744=CARTESIAN_POINT('Origin',(6.,-4.,1.9));
#17745=CARTESIAN_POINT('Origin',(6.,-4.,1.9));
#17746=CARTESIAN_POINT('',(4.5,-4.,2.6));
#17747=CARTESIAN_POINT('Origin',(6.,-4.,2.6));
#17748=CARTESIAN_POINT('',(4.5,-4.,1.9));
#17749=CARTESIAN_POINT('',(4.5,-4.,1.9));
#17750=CARTESIAN_POINT('Origin',(6.,-4.,1.9));
#17751=CARTESIAN_POINT('Origin',(6.,-4.,2.6));
#17752=CARTESIAN_POINT('Origin',(6.,-4.,1.9));
#17753=CARTESIAN_POINT('',(0.,0.,0.));
#17754=CARTESIAN_POINT('Ctrl Pts',(6.99999815899365,-3.98632452652653,2.60093950625054));
#17755=CARTESIAN_POINT('Ctrl Pts',(6.99997288064459,-3.79855038269031,2.62686205390176));
#17756=CARTESIAN_POINT('Ctrl Pts',(6.89233514047511,-3.42414397295474,2.67881370715146));
#17757=CARTESIAN_POINT('Ctrl Pts',(6.45271448161715,-3.02998089899105,2.757384351524));
#17758=CARTESIAN_POINT('Ctrl Pts',(5.86671979479608,-2.93006055988124,2.83651312593273));
#17759=CARTESIAN_POINT('Ctrl Pts',(5.31329781017118,-3.15858496371257,2.91622300969429));
#17760=CARTESIAN_POINT('Ctrl Pts',(4.9638387202763,-3.65012742948249,2.99648818069946));
#17761=CARTESIAN_POINT('Ctrl Pts',(4.9293710419426,-4.25616717719541,3.07729927110974));
#17762=CARTESIAN_POINT('Ctrl Pts',(5.22419213535424,-4.79140012919127,3.15863486906283));
#17763=CARTESIAN_POINT('Ctrl Pts',(5.76222069265107,-5.08919945404236,3.24047453667969));
#17764=CARTESIAN_POINT('Ctrl Pts',(6.379677030618,-5.05504702300603,3.32279319426342));
#17765=CARTESIAN_POINT('Ctrl Pts',(6.88712884688249,-4.6955749219134,3.40556355651458));
#17766=CARTESIAN_POINT('Ctrl Pts',(7.12670085302573,-4.11831918936923,3.48875539197247));
#17767=CARTESIAN_POINT('Ctrl Pts',(7.02192637673817,-3.49920475943206,3.57233609217612));
#17768=CARTESIAN_POINT('Ctrl Pts',(6.60200480535371,-3.02877356919622,3.65627071403784));
#17769=CARTESIAN_POINT('Ctrl Pts',(5.99389696970595,-2.85326346917548,3.74052223770667));
#17770=CARTESIAN_POINT('Ctrl Pts',(5.38356210524816,-3.02876561374954,3.82505176545516));
#17771=CARTESIAN_POINT('Ctrl Pts',(4.97486808401256,-3.48597581907603,3.90667922332894));
#17772=CARTESIAN_POINT('Ctrl Pts',(4.87764331063032,-3.96854834063101,3.97275270796177));
#17773=CARTESIAN_POINT('Ctrl Pts',(4.93363491104256,-4.28466096216571,4.01685604464165));
#17774=CARTESIAN_POINT('Ctrl Pts',(4.99817931143911,-4.45530970670709,4.04207155735716));
#17775=CARTESIAN_POINT('Ctrl Pts',(5.12597275373369,-4.69744865131441,4.07990746653167));
#17776=CARTESIAN_POINT('Ctrl Pts',(5.42875069944469,-4.99309340796393,4.13670511444809));
#17777=CARTESIAN_POINT('Ctrl Pts',(5.97231920216535,-5.14605898976926,4.21249748606625));
#17778=CARTESIAN_POINT('Ctrl Pts',(6.52320508223107,-5.02044374257342,4.28832048254892));
#17779=CARTESIAN_POINT('Ctrl Pts',(6.91110467076896,-4.67743260856581,4.35782392841035));
#17780=CARTESIAN_POINT('Ctrl Pts',(7.09644745188598,-4.25185787791867,4.42098501720712));
#17781=CARTESIAN_POINT('Ctrl Pts',(7.11227598252982,-3.83457932502243,4.47779828333078));
#17782=CARTESIAN_POINT('Ctrl Pts',(6.97422198867159,-3.44096105119827,4.53456659991209));
#17783=CARTESIAN_POINT('Ctrl Pts',(6.67241777459347,-3.08955752755044,4.59757801617794));
#17784=CARTESIAN_POINT('Ctrl Pts',(6.20242890124212,-2.8776477149725,4.66678930738527));
#17785=CARTESIAN_POINT('Ctrl Pts',(5.64251878205079,-2.91980762281901,4.74213608937642));
#17786=CARTESIAN_POINT('Ctrl Pts',(5.2704159386044,-3.1605530148329,4.80163845364204));
#17787=CARTESIAN_POINT('Ctrl Pts',(5.0774166278585,-3.41255654376288,4.84539629257686));
#17788=CARTESIAN_POINT('Ctrl Pts',(4.95479769651029,-3.65506677262475,4.88286085266752));
#17789=CARTESIAN_POINT('Ctrl Pts',(4.89096164216428,-3.99267527518354,4.9296088561907));
#17790=CARTESIAN_POINT('Ctrl Pts',(4.9676452372308,-4.39667000889553,4.98556279567646));
#17791=CARTESIAN_POINT('Ctrl Pts',(5.18583996189851,-4.74396038265063,5.04136211338706));
#17792=CARTESIAN_POINT('Ctrl Pts',(5.51489715544512,-4.98648283834255,5.09699623582978));
#17793=CARTESIAN_POINT('Ctrl Pts',(5.90877797642046,-5.0921366099034,5.15245506500268));
#17794=CARTESIAN_POINT('Ctrl Pts',(6.31208382647452,-5.04618505638536,5.20772889790527));
#17795=CARTESIAN_POINT('Ctrl Pts',(6.79039563711824,-4.79482787477752,5.28116853494519));
#17796=CARTESIAN_POINT('Ctrl Pts',(7.14364250607538,-4.18339760328549,5.37246079320281));
#17797=CARTESIAN_POINT('Ctrl Pts',(6.95465392442801,-3.3615290602033,5.48113680479085));
#17798=CARTESIAN_POINT('Ctrl Pts',(6.37954281770185,-2.97211167108618,5.57092649504958));
#17799=CARTESIAN_POINT('Ctrl Pts',(5.85508217241069,-2.95446460563552,5.64227218334414));
#17800=CARTESIAN_POINT('Ctrl Pts',(5.44460306454923,-3.0974244576334,5.70145206942602));
#17801=CARTESIAN_POINT('Ctrl Pts',(5.09938139322235,-3.43453521092238,5.76619150122483));
#17802=CARTESIAN_POINT('Ctrl Pts',(4.94592320318296,-3.93442474869926,5.83636208316637));
#17803=CARTESIAN_POINT('Ctrl Pts',(5.03197265676116,-4.35840627465708,5.89445465107149));
#17804=CARTESIAN_POINT('Ctrl Pts',(5.19219264369348,-4.60564299044654,5.93491706685731));
#17805=CARTESIAN_POINT('Ctrl Pts',(5.30719577297855,-4.72651611720447,5.95798055540973));
#17806=CARTESIAN_POINT('Ctrl Pts',(5.50053046023923,-4.88495348501329,5.99251787759586));
#17807=CARTESIAN_POINT('Ctrl Pts',(5.85832951556707,-5.02507253962729,6.04410658286047));
#17808=CARTESIAN_POINT('Ctrl Pts',(6.32126493019694,-4.96668267597821,6.10673564915363));
#17809=CARTESIAN_POINT('Ctrl Pts',(6.67328517320073,-4.74489735077078,6.1633365491453));
#17810=CARTESIAN_POINT('Ctrl Pts',(6.89435900913716,-4.44516759248262,6.21402149084589));
#17811=CARTESIAN_POINT('Ctrl Pts',(6.99016055458223,-4.08705298460299,6.26445344730346));
#17812=CARTESIAN_POINT('Ctrl Pts',(6.94870527391535,-3.72056310115263,6.31463598339954));
#17813=CARTESIAN_POINT('Ctrl Pts',(6.77696548585144,-3.39623351183634,6.36457330966794));
#17814=CARTESIAN_POINT('Ctrl Pts',(6.50006848678236,-3.15797695360399,6.41427030439494));
#17815=CARTESIAN_POINT('Ctrl Pts',(6.15689079921747,-3.03828948600061,6.46373243937456));
#17816=CARTESIAN_POINT('Ctrl Pts',(5.73494713487383,-3.05387392617641,6.52117143017342));
#17817=CARTESIAN_POINT('Ctrl Pts',(5.30575107583077,-3.29070893773119,6.58644590514151));
#17818=CARTESIAN_POINT('Ctrl Pts',(5.04125313845857,-3.77122732190886,6.6594050878354));
#17819=CARTESIAN_POINT('Ctrl Pts',(5.06714113786846,-4.2240700226978,6.71983222627245));
#17820=CARTESIAN_POINT('Ctrl Pts',(5.22896371026909,-4.53583531846688,6.76796591127916));
#17821=CARTESIAN_POINT('Ctrl Pts',(5.42916113979845,-4.74785467675554,6.80796630808184));
#17822=CARTESIAN_POINT('Ctrl Pts',(5.714367370309,-4.89850759732021,6.85183024025803));
#17823=CARTESIAN_POINT('Ctrl Pts',(6.06253639457921,-4.93755475445945,6.89952195690528));
#17824=CARTESIAN_POINT('Ctrl Pts',(6.4565847787629,-4.83233977440753,6.95498839066731));
#17825=CARTESIAN_POINT('Ctrl Pts',(6.81022730237302,-4.51633849133825,7.01814871600544));
#17826=CARTESIAN_POINT('Ctrl Pts',(6.95706828830077,-4.00489886911992,7.08893287981098));
#17827=CARTESIAN_POINT('Ctrl Pts',(6.81021224891959,-3.49584469103884,7.15948666255227));
#17828=CARTESIAN_POINT('Ctrl Pts',(6.41592301667082,-3.14352189275395,7.22985222727915));
#17829=CARTESIAN_POINT('Ctrl Pts',(5.89582428767248,-3.0555832223308,7.30007283378182));
#17830=CARTESIAN_POINT('Ctrl Pts',(5.40914881608276,-3.25711226719962,7.37019262219717));
#17831=CARTESIAN_POINT('Ctrl Pts',(5.10471600640629,-3.68647088534127,7.4402563254545));
#17832=CARTESIAN_POINT('Ctrl Pts',(5.07493689936822,-4.21187381141773,7.51030900528994));
#17833=CARTESIAN_POINT('Ctrl Pts',(5.32972438815395,-4.67276168571651,7.58039577687912));
#17834=CARTESIAN_POINT('Ctrl Pts',(5.79102554371443,-4.92784792737786,7.65056157421906));
#17835=CARTESIAN_POINT('Ctrl Pts',(6.31826031255578,-4.89837953861158,7.72085085714204));
#17836=CARTESIAN_POINT('Ctrl Pts',(6.75020660471299,-4.59231290695902,7.79130734550421));
#17837=CARTESIAN_POINT('Ctrl Pts',(6.95334524231267,-4.10180979072915,7.86197377515194));
#17838=CARTESIAN_POINT('Ctrl Pts',(6.86452811856373,-3.57660445666216,7.93289164673106));
#17839=CARTESIAN_POINT('Ctrl Pts',(6.50822949801913,-3.17741851765368,8.00410096472273));
#17840=CARTESIAN_POINT('Ctrl Pts',(5.99202912111436,-3.02846879700038,8.07564001126929));
#17841=CARTESIAN_POINT('Ctrl Pts',(5.47262775862424,-3.1772786287127,8.14754510192845));
#17842=CARTESIAN_POINT('Ctrl Pts',(5.12396773984527,-3.56713104102442,8.21717245978697));
#17843=CARTESIAN_POINT('Ctrl Pts',(5.02465088008016,-4.0589090579052,8.28449962671212));
#17844=CARTESIAN_POINT('Ctrl Pts',(5.16664179671633,-4.52183049710153,8.34949563002517));
#17845=CARTESIAN_POINT('Ctrl Pts',(5.48622133819085,-4.83366725020512,8.40942447534479));
#17846=CARTESIAN_POINT('Ctrl Pts',(5.86625745021743,-4.9665851067969,8.4641954747342));
#17847=CARTESIAN_POINT('Ctrl Pts',(6.22997586892847,-4.95324406413884,8.5137197914407));
#17848=CARTESIAN_POINT('Ctrl Pts',(6.56523678307791,-4.80705258085916,8.56348049146453));
#17849=CARTESIAN_POINT('Ctrl Pts',(6.8252178463785,-4.54733568382595,8.61348288991823));
#17850=CARTESIAN_POINT('Ctrl Pts',(6.97306928054101,-4.20890471076454,8.6637316832973));
#17851=CARTESIAN_POINT('Ctrl Pts',(6.98712341108126,-3.83802816814003,8.7142309149468));
#17852=CARTESIAN_POINT('Ctrl Pts',(6.86409431800442,-3.4858887373625,8.76498396878373));
#17853=CARTESIAN_POINT('Ctrl Pts',(6.61968641501593,-3.20161333099039,8.81599356080702));
#17854=CARTESIAN_POINT('Ctrl Pts',(6.28663539552411,-3.02539046352671,8.8672617337013));
#17855=CARTESIAN_POINT('Ctrl Pts',(5.91032079687008,-2.98281618785264,8.9187898484193));
#17856=CARTESIAN_POINT('Ctrl Pts',(5.54261902100133,-3.08115683102349,8.97057858319571));
#17857=CARTESIAN_POINT('Ctrl Pts',(5.23470149593991,-3.30818973404657,9.02262792887906));
#17858=CARTESIAN_POINT('Ctrl Pts',(5.03002953653242,-3.63360637314209,9.07493719454492));
#17859=CARTESIAN_POINT('Ctrl Pts',(4.95795339049146,-4.01324887545392,9.12750499722226));
#17860=CARTESIAN_POINT('Ctrl Pts',(5.03008733681497,-4.39465616925505,9.18032929191999));
#17861=CARTESIAN_POINT('Ctrl Pts',(5.26037098227884,-4.76198737973904,9.23930488376548));
#17862=CARTESIAN_POINT('Ctrl Pts',(5.66815402132354,-5.02611715334513,9.30453505328307));
#17863=CARTESIAN_POINT('Ctrl Pts',(6.20031175950905,-5.06610553161693,9.37613052247429));
#17864=CARTESIAN_POINT('Ctrl Pts',(6.57211483447548,-4.89867154701958,9.43089482659667));
#17865=CARTESIAN_POINT('Ctrl Pts',(6.77268428325753,-4.71398594666241,9.46854124254023));
#17866=CARTESIAN_POINT('Ctrl Pts',(6.89732261541234,-4.56210906285714,9.4956893772699));
#17867=CARTESIAN_POINT('Ctrl Pts',(7.05743952416135,-4.25373892219051,9.54330952558428));
#17868=CARTESIAN_POINT('Ctrl Pts',(7.08681427060224,-3.7413976498585,9.61164803498953));
#17869=CARTESIAN_POINT('Ctrl Pts',(6.78743967682059,-3.19877575055479,9.69412425474241));
#17870=CARTESIAN_POINT('Ctrl Pts',(6.24245837315985,-2.89706443193603,9.77704206668623));
#17871=CARTESIAN_POINT('Ctrl Pts',(5.61746900273164,-2.93185417099466,9.86037047868398));
#17872=CARTESIAN_POINT('Ctrl Pts',(5.1042042416184,-3.29518411512121,9.94407604361117));
#17873=CARTESIAN_POINT('Ctrl Pts',(4.86233946758306,-3.8785536270643,10.0281231251224));
#17874=CARTESIAN_POINT('Ctrl Pts',(4.96816269898698,-4.50332086698013,10.1124740074888));
#17875=CARTESIAN_POINT('Ctrl Pts',(5.3915816199262,-4.97752738430232,10.1970892227568));
#17876=CARTESIAN_POINT('Ctrl Pts',(6.00397807691952,-5.15417755509278,10.281927720062));
#17877=CARTESIAN_POINT('Ctrl Pts',(6.61779621608409,-4.97752665860305,10.3669471357688));
#17878=CARTESIAN_POINT('Ctrl Pts',(7.04418758947222,-4.50057596349951,10.4521040140405));
#17879=CARTESIAN_POINT('Ctrl Pts',(7.15154318711507,-3.86917823804319,10.5373541207604));
#17880=CARTESIAN_POINT('Ctrl Pts',(6.9063217242137,-3.27712490715728,10.622652644332));
#17881=CARTESIAN_POINT('Ctrl Pts',(6.38365961018741,-2.90630232377856,10.70795449752));
#17882=CARTESIAN_POINT('Ctrl Pts',(5.74407957751689,-2.87046702674317,10.7932145497474));
#17883=CARTESIAN_POINT('Ctrl Pts',(5.18413779010185,-3.18009512220889,10.8783879953558));
#17884=CARTESIAN_POINT('Ctrl Pts',(4.87504525063398,-3.73939474085648,10.9634303821887));
#17885=CARTESIAN_POINT('Ctrl Pts',(4.9113280193628,-4.37593360867611,11.0482983399598));
#17886=CARTESIAN_POINT('Ctrl Pts',(5.27937248430205,-4.89450749674953,11.1329488708158));
#17887=CARTESIAN_POINT('Ctrl Pts',(5.86527624347711,-5.13679808752952,11.2173417295453));
#17888=CARTESIAN_POINT('Ctrl Pts',(6.48799534199112,-5.03087191620999,11.3014349903219));
#17889=CARTESIAN_POINT('Ctrl Pts',(6.95693136473707,-4.61090781293032,11.3851957485584));
#17890=CARTESIAN_POINT('Ctrl Pts',(7.07219562678886,-4.21035033769926,11.4407823887657));
#17891=CARTESIAN_POINT('Ctrl Pts',(7.07222266979228,-4.00946826992833,11.4685145081909));
#17892=CARTESIAN_POINT('Ctrl Pts',(6.97007822923057,-3.98632855437836,2.60093950625054));
#17893=CARTESIAN_POINT('Ctrl Pts',(6.97005368434428,-3.80400276250044,2.62610989942311));
#17894=CARTESIAN_POINT('Ctrl Pts',(6.8655981616237,-3.44058276592777,2.67653039560817));
#17895=CARTESIAN_POINT('Ctrl Pts',(6.43867935390673,-3.05771294402619,2.75283688635242));
#17896=CARTESIAN_POINT('Ctrl Pts',(5.86925370182103,-2.96056862970221,2.829722772863));
#17897=CARTESIAN_POINT('Ctrl Pts',(5.33104067083453,-3.18273229632189,2.90723423398096));
#17898=CARTESIAN_POINT('Ctrl Pts',(4.99083036824212,-3.6611258102588,2.98535322301203));
#17899=CARTESIAN_POINT('Ctrl Pts',(4.95715560557959,-4.25162171008957,3.06408756320453));
#17900=CARTESIAN_POINT('Ctrl Pts',(5.24465534103322,-4.77378946224153,3.14342202919564));
#17901=CARTESIAN_POINT('Ctrl Pts',(5.77010719210167,-5.06476100581107,3.22334344667496));
#17902=CARTESIAN_POINT('Ctrl Pts',(6.37406294588003,-5.0314844936736,3.30385018064892));
#17903=CARTESIAN_POINT('Ctrl Pts',(6.87124480480666,-4.67945377128695,3.38491957776513));
#17904=CARTESIAN_POINT('Ctrl Pts',(7.10644641749634,-4.11311294816235,3.46653370137737));
#17905=CARTESIAN_POINT('Ctrl Pts',(7.00362219975504,-3.50458520131084,3.54866794881851));
#17906=CARTESIAN_POINT('Ctrl Pts',(6.59028971235191,-3.04128632982343,3.63129605781087));
#17907=CARTESIAN_POINT('Ctrl Pts',(5.9904902635316,-2.86799412215644,3.71438857179753));
#17908=CARTESIAN_POINT('Ctrl Pts',(5.38725457312936,-3.04126659406085,3.79791248632923));
#17909=CARTESIAN_POINT('Ctrl Pts',(4.98243162058577,-3.49388688470476,3.87872607649656));
#17910=CARTESIAN_POINT('Ctrl Pts',(4.88586987972222,-3.97261107956554,3.94426166404564));
#17911=CARTESIAN_POINT('Ctrl Pts',(4.94147690622331,-4.28666010423245,3.9880717841222));
#17912=CARTESIAN_POINT('Ctrl Pts',(5.00564118171601,-4.45631175436491,4.01313856907925));
#17913=CARTESIAN_POINT('Ctrl Pts',(5.13273792342617,-4.69714409310281,4.05076810237111));
#17914=CARTESIAN_POINT('Ctrl Pts',(5.43409624307086,-4.99155886825263,4.10729667550138));
#17915=CARTESIAN_POINT('Ctrl Pts',(5.97628316486736,-5.1442798788599,4.18289693437406));
#17916=CARTESIAN_POINT('Ctrl Pts',(6.52681800343661,-5.01887678936212,4.25865819770454));
#17917=CARTESIAN_POINT('Ctrl Pts',(6.91522840587363,-4.67558077820218,4.32822383176324));
#17918=CARTESIAN_POINT('Ctrl Pts',(7.10113200959162,-4.24885108696776,4.39155418341742));
#17919=CARTESIAN_POINT('Ctrl Pts',(7.11708265563879,-3.82987437918727,4.44859070552638));
#17920=CARTESIAN_POINT('Ctrl Pts',(6.97831413390946,-3.43409394973361,4.50566173126832));
#17921=CARTESIAN_POINT('Ctrl Pts',(6.6745131582099,-3.08027116188779,4.56909239590932));
#17922=CARTESIAN_POINT('Ctrl Pts',(6.2006354612538,-2.86648985101506,4.63887572589507));
#17923=CARTESIAN_POINT('Ctrl Pts',(5.63505204541033,-2.90895569779608,4.71498055830681));
#17924=CARTESIAN_POINT('Ctrl Pts',(5.25855479608114,-3.15244878707084,4.77515896552872));
#17925=CARTESIAN_POINT('Ctrl Pts',(5.06304540191057,-3.4077178457721,4.81948131645844));
#17926=CARTESIAN_POINT('Ctrl Pts',(4.93875890697152,-3.65351683513821,4.85745130169426));
#17927=CARTESIAN_POINT('Ctrl Pts',(4.87395928312855,-3.99601029957039,4.9048726153362));
#17928=CARTESIAN_POINT('Ctrl Pts',(4.95180908604431,-4.40634593719688,4.961698237853));
#17929=CARTESIAN_POINT('Ctrl Pts',(5.17363722686749,-4.75950452494967,5.01843134223497));
#17930=CARTESIAN_POINT('Ctrl Pts',(5.50858725429261,-5.00640760956707,5.07505875580519));
#17931=CARTESIAN_POINT('Ctrl Pts',(5.90996241751456,-5.11411410956675,5.13157061683935));
#17932=CARTESIAN_POINT('Ctrl Pts',(6.32138714457423,-5.0672664088841,5.18795230177275));
#17933=CARTESIAN_POINT('Ctrl Pts',(6.80982170387704,-4.81064962531081,5.26294063889726));
#17934=CARTESIAN_POINT('Ctrl Pts',(7.17122043266886,-4.18554904460768,5.35628142326472));
#17935=CARTESIAN_POINT('Ctrl Pts',(6.97788741209539,-3.34365221835195,5.4675913947686));
#17936=CARTESIAN_POINT('Ctrl Pts',(6.38801757398717,-2.94404847700065,5.55969225114999));
#17937=CARTESIAN_POINT('Ctrl Pts',(5.84950720702512,-2.92590597485546,5.63294592890857));
#17938=CARTESIAN_POINT('Ctrl Pts',(5.42780119252992,-3.07275825516153,5.69374335618479));
#17939=CARTESIAN_POINT('Ctrl Pts',(5.07291053225168,-3.41926575125888,5.76029097754461));
#17940=CARTESIAN_POINT('Ctrl Pts',(4.91505669962947,-3.93339958881015,5.83246170467108));
#17941=CARTESIAN_POINT('Ctrl Pts',(5.00358120253044,-4.36965344538107,5.89223592257864));
#17942=CARTESIAN_POINT('Ctrl Pts',(5.16847877874769,-4.62410237756779,5.93387965098663));
#17943=CARTESIAN_POINT('Ctrl Pts',(5.28684674764252,-4.74851097849003,5.95761805778754));
#17944=CARTESIAN_POINT('Ctrl Pts',(5.48584905677489,-4.91159032288957,5.99316834802937));
#17945=CARTESIAN_POINT('Ctrl Pts',(5.85417679119542,-5.0558315382256,6.04627671719175));
#17946=CARTESIAN_POINT('Ctrl Pts',(6.33075428932811,-4.99570908084568,6.11075504563264));
#17947=CARTESIAN_POINT('Ctrl Pts',(6.69311737100275,-4.76738932049588,6.16902548955981));
#17948=CARTESIAN_POINT('Ctrl Pts',(6.92063937745368,-4.45890309164721,6.22119126264878));
#17949=CARTESIAN_POINT('Ctrl Pts',(7.01920463848466,-4.0904003195319,6.27308960467507));
#17950=CARTESIAN_POINT('Ctrl Pts',(6.97654392840764,-3.71341013806137,6.32471316097078));
#17951=CARTESIAN_POINT('Ctrl Pts',(6.79993515733336,-3.37991978141767,6.37606575989576));
#17952=CARTESIAN_POINT('Ctrl Pts',(6.51532665733549,-3.13506167065285,6.42714817101994));
#17953=CARTESIAN_POINT('Ctrl Pts',(6.16279711837762,-3.01213654187887,6.47796294003246));
#17954=CARTESIAN_POINT('Ctrl Pts',(5.72964410429838,-3.02816623710855,6.53693063505321));
#17955=CARTESIAN_POINT('Ctrl Pts',(5.28944670857787,-3.27117558494452,6.60389777235902));
#17956=CARTESIAN_POINT('Ctrl Pts',(5.0185771110185,-3.76349640673093,6.67865338334697));
#17957=CARTESIAN_POINT('Ctrl Pts',(5.04515925875904,-4.22673789405818,6.74047442293565));
#17958=CARTESIAN_POINT('Ctrl Pts',(5.21052884288523,-4.54528741933717,6.78966498160772));
#17959=CARTESIAN_POINT('Ctrl Pts',(5.41493563316234,-4.7617396587125,6.83050795551897));
#17960=CARTESIAN_POINT('Ctrl Pts',(5.70585879542675,-4.91537056653778,6.87525779471725));
#17961=CARTESIAN_POINT('Ctrl Pts',(6.06053583697364,-4.95510732388249,6.92384372352008));
#17962=CARTESIAN_POINT('Ctrl Pts',(6.46143918692318,-4.84800603500354,6.98028564004111));
#17963=CARTESIAN_POINT('Ctrl Pts',(6.82054812942106,-4.52694081115451,7.04444324737071));
#17964=CARTESIAN_POINT('Ctrl Pts',(6.96921975414278,-4.00847570947695,7.11621410834575));
#17965=CARTESIAN_POINT('Ctrl Pts',(6.82053287811316,-3.49368195718114,7.18758462714898));
#17966=CARTESIAN_POINT('Ctrl Pts',(6.42254980324896,-3.13829762703421,7.25860889560072));
#17967=CARTESIAN_POINT('Ctrl Pts',(5.89899472566348,-3.04994843752126,7.32930394453428));
#17968=CARTESIAN_POINT('Ctrl Pts',(5.4103834061862,-3.2524805765858,7.3997215654219));
#17969=CARTESIAN_POINT('Ctrl Pts',(5.10560112805102,-3.68264223188015,7.46990822314288));
#17970=CARTESIAN_POINT('Ctrl Pts',(5.07603810075024,-4.20761021857705,7.53991183200612));
#17971=CARTESIAN_POINT('Ctrl Pts',(5.33014059158489,-4.66688873918372,7.60978622792386));
#17972=CARTESIAN_POINT('Ctrl Pts',(5.7888549752637,-4.9203345943961,7.67956006945411));
#17973=CARTESIAN_POINT('Ctrl Pts',(6.31174238725869,-4.89093964456828,7.74928634435711));
#17974=CARTESIAN_POINT('Ctrl Pts',(6.73902593000717,-4.58796385083579,7.81901619775126));
#17975=CARTESIAN_POINT('Ctrl Pts',(6.93939676985519,-4.10372565119263,7.88878272235039));
#17976=CARTESIAN_POINT('Ctrl Pts',(6.851762373771,-3.58646485209147,7.95863747128128));
#17977=CARTESIAN_POINT('Ctrl Pts',(6.50145440276794,-3.1942196339742,8.02863622738192));
#17978=CARTESIAN_POINT('Ctrl Pts',(5.99506812255964,-3.04824066370828,8.09881519965856));
#17979=CARTESIAN_POINT('Ctrl Pts',(5.48652398303505,-3.19407539673001,8.16923214994343));
#17980=CARTESIAN_POINT('Ctrl Pts',(5.14580163911575,-3.57521396317503,8.23729514829861));
#17981=CARTESIAN_POINT('Ctrl Pts',(5.04892012023588,-4.0552555450462,8.30302386698914));
#17982=CARTESIAN_POINT('Ctrl Pts',(5.18740669602069,-4.50653622748511,8.36639189808384));
#17983=CARTESIAN_POINT('Ctrl Pts',(5.4986550261764,-4.81018052115883,8.42475683928535));
#17984=CARTESIAN_POINT('Ctrl Pts',(5.86844941776158,-4.93949335407164,8.4780524865146));
#17985=CARTESIAN_POINT('Ctrl Pts',(6.22215032474989,-4.9265097772033,8.52621674759037));
#17986=CARTESIAN_POINT('Ctrl Pts',(6.54798916354433,-4.7844123100289,8.57458080609539));
#17987=CARTESIAN_POINT('Ctrl Pts',(6.80055242150616,-4.53209565232151,8.62315924176611));
#17988=CARTESIAN_POINT('Ctrl Pts',(6.94413060607835,-4.2034339501668,8.67195830251317));
#17989=CARTESIAN_POINT('Ctrl Pts',(6.95777336420282,-3.84336797794748,8.72098623179676));
#17990=CARTESIAN_POINT('Ctrl Pts',(6.83835542549463,-3.50156151069008,8.77025013770849));
#17991=CARTESIAN_POINT('Ctrl Pts',(6.60115058604047,-3.22565815234949,8.81975670172189));
#17992=CARTESIAN_POINT('Ctrl Pts',(6.27792608816288,-3.05462702721105,8.86951191522505));
#17993=CARTESIAN_POINT('Ctrl Pts',(5.91269587682919,-3.01329689282491,8.91952105747049));
#17994=CARTESIAN_POINT('Ctrl Pts',(5.55577670770468,-3.10874082258239,8.96978893051619));
#17995=CARTESIAN_POINT('Ctrl Pts',(5.25682184453666,-3.32914518984797,9.02031918435157));
#17996=CARTESIAN_POINT('Ctrl Pts',(5.05804379683145,-3.6451580106137,9.07111583459068));
#17997=CARTESIAN_POINT('Ctrl Pts',(4.98800203972588,-4.01396234221588,9.12217980455873));
#17998=CARTESIAN_POINT('Ctrl Pts',(5.0580876534622,-4.38465341916386,9.17351671572958));
#17999=CARTESIAN_POINT('Ctrl Pts',(5.2819853526548,-4.74184810488963,9.23085986274571));
#18000=CARTESIAN_POINT('Ctrl Pts',(5.67872943927656,-4.99889438490076,9.29432501935413));
#18001=CARTESIAN_POINT('Ctrl Pts',(6.19695075641161,-5.03790457902352,9.36403899527298));
#18002=CARTESIAN_POINT('Ctrl Pts',(6.55940562763933,-4.87474206041059,9.41741918235656));
#18003=CARTESIAN_POINT('Ctrl Pts',(6.75506127473338,-4.69458762928485,9.45414031901828));
#18004=CARTESIAN_POINT('Ctrl Pts',(6.87668522837596,-4.54638877836258,9.48063024933242));
#18005=CARTESIAN_POINT('Ctrl Pts',(7.03301072347723,-4.245368303688,9.52711237127836));
#18006=CARTESIAN_POINT('Ctrl Pts',(7.06181762289588,-3.74471411884191,9.59388652174575));
#18007=CARTESIAN_POINT('Ctrl Pts',(6.7689591760146,-3.21363601446678,9.67459068366522));
#18008=CARTESIAN_POINT('Ctrl Pts',(6.23487010697712,-2.91779656590466,9.75585247155239));
#18009=CARTESIAN_POINT('Ctrl Pts',(5.62127050868205,-2.95181143891995,9.83765382096644));
#18010=CARTESIAN_POINT('Ctrl Pts',(5.11641195631316,-3.30899758881283,9.91996355293717));
#18011=CARTESIAN_POINT('Ctrl Pts',(4.87798505278271,-3.8836659287957,10.0027473525134));
#18012=CARTESIAN_POINT('Ctrl Pts',(4.98227272841176,-4.50036948740507,10.0859920067241));
#18013=CARTESIAN_POINT('Ctrl Pts',(5.40088585422602,-4.96944698093703,10.1696561496146));
#18014=CARTESIAN_POINT('Ctrl Pts',(6.00765739583399,-5.14465807361536,10.2537075984136));
#18015=CARTESIAN_POINT('Ctrl Pts',(6.61715595103273,-4.96943730503454,10.3381068322003));
#18016=CARTESIAN_POINT('Ctrl Pts',(7.04150787840671,-4.49504167195355,10.4228145333172));
#18017=CARTESIAN_POINT('Ctrl Pts',(7.14871630829242,-3.86560883063579,10.5077887784152));
#18018=CARTESIAN_POINT('Ctrl Pts',(6.90391357861512,-3.27408223567318,10.5929860562277));
#18019=CARTESIAN_POINT('Ctrl Pts',(6.38081263394418,-2.90272063471259,10.6783623214699));
#18020=CARTESIAN_POINT('Ctrl Pts',(5.73926233026402,-2.86658474978731,10.7638702346137));
#18021=CARTESIAN_POINT('Ctrl Pts',(5.17635857755646,-3.17764139675116,10.849466654309));
#18022=CARTESIAN_POINT('Ctrl Pts',(4.86489677958424,-3.74082925476046,10.9350964140044));
#18023=CARTESIAN_POINT('Ctrl Pts',(4.90133545189447,-4.383198400959,11.0207291628158));
#18024=CARTESIAN_POINT('Ctrl Pts',(5.27331123911313,-4.90761852821718,11.1063112487012));
#18025=CARTESIAN_POINT('Ctrl Pts',(5.8667411442123,-5.15320882638912,11.1917885764413));
#18026=CARTESIAN_POINT('Ctrl Pts',(6.49868316645557,-5.0458533596991,11.2771194094233));
#18027=CARTESIAN_POINT('Ctrl Pts',(6.97547246984522,-4.61907226633235,11.3622555926326));
#18028=CARTESIAN_POINT('Ctrl Pts',(7.09288943197313,-4.21115651665385,11.4188571787892));
#18029=CARTESIAN_POINT('Ctrl Pts',(7.09291698096071,-4.0065158743674,11.4471081759743));
#18030=CARTESIAN_POINT('Ctrl Pts',(6.91041388003776,-3.99025785493753,2.62934384528526));
#18031=CARTESIAN_POINT('Ctrl Pts',(6.91039080704782,-3.81886569155907,2.65300483199757));
#18032=CARTESIAN_POINT('Ctrl Pts',(6.8122491622858,-3.47775408576118,2.70033480637834));
#18033=CARTESIAN_POINT('Ctrl Pts',(6.41196409991056,-3.11888567055589,2.77187288605298));
#18034=CARTESIAN_POINT('Ctrl Pts',(5.87870459195709,-3.02800305041287,2.84387354450334));
#18035=CARTESIAN_POINT('Ctrl Pts',(5.37501897776042,-3.23595938105673,2.91641672576983));
#18036=CARTESIAN_POINT('Ctrl Pts',(5.05670377179691,-3.68359061413889,2.98951226441559));
#18037=CARTESIAN_POINT('Ctrl Pts',(5.02516628278399,-4.23620154296935,3.06319721265735));
#18038=CARTESIAN_POINT('Ctrl Pts',(5.29433269147969,-4.72517576991202,3.13748867038598));
#18039=CARTESIAN_POINT('Ctrl Pts',(5.78679871047612,-4.99797595495716,3.21240611140967));
#18040=CARTESIAN_POINT('Ctrl Pts',(6.35363537824581,-4.96685750155159,3.28797094288595));
#18041=CARTESIAN_POINT('Ctrl Pts',(6.8211198508534,-4.63603041178032,3.36419307761376));
#18042=CARTESIAN_POINT('Ctrl Pts',(7.04283368983127,-4.10260934326042,3.4410820879014));
#18043=CARTESIAN_POINT('Ctrl Pts',(6.94594187284151,-3.52801981043285,3.51864207258902));
#18044=CARTESIAN_POINT('Ctrl Pts',(6.55482388157473,-3.08929256377072,3.59687389466955));
#18045=CARTESIAN_POINT('Ctrl Pts',(5.98544482856865,-2.92453923112812,3.67577412964314));
#18046=CARTESIAN_POINT('Ctrl Pts',(5.41085897745953,-3.08930968376791,3.75533558541602));
#18047=CARTESIAN_POINT('Ctrl Pts',(5.02379505335764,-3.52165808238205,3.83257622804987));
#18048=CARTESIAN_POINT('Ctrl Pts',(4.931020522875,-3.98066380798232,3.89542943544965));
#18049=CARTESIAN_POINT('Ctrl Pts',(4.9844408484075,-4.28254645693087,3.93754525316638));
#18050=CARTESIAN_POINT('Ctrl Pts',(5.04619135722488,-4.44582563834565,3.96167148603502));
#18051=CARTESIAN_POINT('Ctrl Pts',(5.16861301581523,-4.67780809698434,3.99792049351659));
#18052=CARTESIAN_POINT('Ctrl Pts',(5.45946253135908,-4.96217671243346,4.05251748479476));
#18053=CARTESIAN_POINT('Ctrl Pts',(5.98468607065537,-5.11036489028024,4.12576694910513));
#18054=CARTESIAN_POINT('Ctrl Pts',(6.52011973324497,-4.98866785198386,4.19945297410707));
#18055=CARTESIAN_POINT('Ctrl Pts',(6.89945162846597,-4.65370085290913,4.26738008926097));
#18056=CARTESIAN_POINT('Ctrl Pts',(7.08165637686814,-4.23578697094255,4.32941453727684));
#18057=CARTESIAN_POINT('Ctrl Pts',(7.09743152418886,-3.82420346898175,4.38545624718568));
#18058=CARTESIAN_POINT('Ctrl Pts',(6.96082001314597,-3.43420568070724,4.44169499055966));
#18059=CARTESIAN_POINT('Ctrl Pts',(6.66069499579344,-3.08446880580411,4.50439011816686));
#18060=CARTESIAN_POINT('Ctrl Pts',(6.19086806115881,-2.87223085510411,4.5736016912126));
#18061=CARTESIAN_POINT('Ctrl Pts',(5.62770576916625,-2.91422420562986,4.64938324638858));
#18062=CARTESIAN_POINT('Ctrl Pts',(5.25111785199374,-3.15750274058377,4.70958190751128));
#18063=CARTESIAN_POINT('Ctrl Pts',(5.05509817427152,-3.41339807779548,4.75401872379404));
#18064=CARTESIAN_POINT('Ctrl Pts',(4.93029391983906,-3.66017056351555,4.79214573005493));
#18065=CARTESIAN_POINT('Ctrl Pts',(4.86499221929501,-4.0048010675327,4.83987165496948));
#18066=CARTESIAN_POINT('Ctrl Pts',(4.94344411857747,-4.41899208362928,4.89723533807431));
#18067=CARTESIAN_POINT('Ctrl Pts',(5.16791520878115,-4.77657053811553,4.954677607837));
#18068=CARTESIAN_POINT('Ctrl Pts',(5.50792791889865,-5.02736403777264,5.01218255346116));
#18069=CARTESIAN_POINT('Ctrl Pts',(5.91660949347755,-5.13715603053052,5.06973457806084));
#18070=CARTESIAN_POINT('Ctrl Pts',(6.3367779644244,-5.08942543737139,5.12731888318447));
#18071=CARTESIAN_POINT('Ctrl Pts',(6.83702927977863,-4.82679209842469,5.20411951082081));
#18072=CARTESIAN_POINT('Ctrl Pts',(7.20933766937117,-4.18431587015626,5.30013430054567));
#18073=CARTESIAN_POINT('Ctrl Pts',(7.01034570705962,-3.31366155048617,5.41523225831058));
#18074=CARTESIAN_POINT('Ctrl Pts',(6.3977364131714,-2.89784267685387,5.5109554305934));
#18075=CARTESIAN_POINT('Ctrl Pts',(5.83613927351209,-2.87878248811417,5.58735163070686));
#18076=CARTESIAN_POINT('Ctrl Pts',(5.39535814415608,-3.03217873181673,5.65090114175908));
#18077=CARTESIAN_POINT('Ctrl Pts',(5.02334729005529,-3.3951294460668,5.72063905656003));
#18078=CARTESIAN_POINT('Ctrl Pts',(4.85728925835324,-3.93530401284747,5.79647914846814));
#18079=CARTESIAN_POINT('Ctrl Pts',(4.95040053000959,-4.3948784892822,5.85944685621913));
#18080=CARTESIAN_POINT('Ctrl Pts',(5.12438570171492,-4.66340933665913,5.90339414657583));
#18081=CARTESIAN_POINT('Ctrl Pts',(5.2493935187274,-4.79480118236336,5.92846496633277));
#18082=CARTESIAN_POINT('Ctrl Pts',(5.4596703719434,-4.96713107722029,5.96603147351556));
#18083=CARTESIAN_POINT('Ctrl Pts',(5.8493603739367,-5.11985609810124,6.02222723777501));
#18084=CARTESIAN_POINT('Ctrl Pts',(6.35460113952391,-5.05624174985086,6.09058222260399));
#18085=CARTESIAN_POINT('Ctrl Pts',(6.73933984369154,-4.81390063965477,6.15244556102042));
#18086=CARTESIAN_POINT('Ctrl Pts',(6.98118457887927,-4.48606318884047,6.20788769925023));
#18087=CARTESIAN_POINT('Ctrl Pts',(7.08608186634963,-4.09405409466647,6.26309751878246));
#18088=CARTESIAN_POINT('Ctrl Pts',(7.04069467998163,-3.69267509562981,6.31805903401915));
#18089=CARTESIAN_POINT('Ctrl Pts',(6.85256366464928,-3.33737104537872,6.3727674879457));
#18090=CARTESIAN_POINT('Ctrl Pts',(6.54921482208544,-3.07635812326129,6.42721377541));
#18091=CARTESIAN_POINT('Ctrl Pts',(6.17333370611417,-2.94527448076034,6.48139220696859));
#18092=CARTESIAN_POINT('Ctrl Pts',(5.71139634990446,-2.96235904620064,6.54427642819304));
#18093=CARTESIAN_POINT('Ctrl Pts',(5.24195855587125,-3.22150171333028,6.61568196044263));
#18094=CARTESIAN_POINT('Ctrl Pts',(4.95324402611607,-3.74634709443177,6.69536386654557));
#18095=CARTESIAN_POINT('Ctrl Pts',(4.98161750117062,-4.23980174957217,6.76121320872448));
#18096=CARTESIAN_POINT('Ctrl Pts',(5.15763242426064,-4.57881842470844,6.81356023789864));
#18097=CARTESIAN_POINT('Ctrl Pts',(5.37504268972789,-4.80902468214805,6.85699616204033));
#18098=CARTESIAN_POINT('Ctrl Pts',(5.68418613989248,-4.97223633786759,6.90453778880486));
#18099=CARTESIAN_POINT('Ctrl Pts',(6.06062183697248,-5.01436815416344,6.95610098888784));
#18100=CARTESIAN_POINT('Ctrl Pts',(6.48550711521371,-4.90080029315905,7.01591156763435));
#18101=CARTESIAN_POINT('Ctrl Pts',(6.86525409936937,-4.56104588973726,7.08377161093949));
#18102=CARTESIAN_POINT('Ctrl Pts',(7.02186082581237,-4.01409341078421,7.15945586805767));
#18103=CARTESIAN_POINT('Ctrl Pts',(6.86526232149639,-3.47282042782154,7.23449212322981));
#18104=CARTESIAN_POINT('Ctrl Pts',(6.44802413959838,-3.10062213493182,7.30889612256709));
#18105=CARTESIAN_POINT('Ctrl Pts',(5.901400424226,-3.00870277543536,7.3826878474804));
#18106=CARTESIAN_POINT('Ctrl Pts',(5.39352039285457,-3.21957437439377,7.45588985731414));
#18107=CARTESIAN_POINT('Ctrl Pts',(5.07833615802819,-3.66503206095406,7.5285291186389));
#18108=CARTESIAN_POINT('Ctrl Pts',(5.04823664994393,-4.20588633168366,7.60063427930656));
#18109=CARTESIAN_POINT('Ctrl Pts',(5.30904925496711,-4.67648866522258,7.67223726675353));
#18110=CARTESIAN_POINT('Ctrl Pts',(5.77705173780209,-4.93462323268497,7.74337645487925));
#18111=CARTESIAN_POINT('Ctrl Pts',(6.30746620650405,-4.90439550306326,7.81409007533856));
#18112=CARTESIAN_POINT('Ctrl Pts',(6.73832012465397,-4.598388527706,7.88441740191195));
#18113=CARTESIAN_POINT('Ctrl Pts',(6.93898456949613,-4.11235148307006,7.95440671960687));
#18114=CARTESIAN_POINT('Ctrl Pts',(6.85113932402579,-3.59626983255766,8.02410221512531));
#18115=CARTESIAN_POINT('Ctrl Pts',(6.50323102966143,-3.20732217322844,8.09354734997649));
#18116=CARTESIAN_POINT('Ctrl Pts',(6.00339991092543,-3.06365063168461,8.16279549808777));
#18117=CARTESIAN_POINT('Ctrl Pts',(5.50439671438939,-3.20715934459842,8.23188849529843));
#18118=CARTESIAN_POINT('Ctrl Pts',(5.17202190935144,-3.57951563299814,8.29833266947451));
#18119=CARTESIAN_POINT('Ctrl Pts',(5.07818019990084,-4.04593165133975,8.36217277635728));
#18120=CARTESIAN_POINT('Ctrl Pts',(5.21238143820554,-4.48240836001952,8.42346320100455));
#18121=CARTESIAN_POINT('Ctrl Pts',(5.51236025777204,-4.77474404476563,8.47967815909619));
#18122=CARTESIAN_POINT('Ctrl Pts',(5.86737823061201,-4.89877834106162,8.53083636744996));
#18123=CARTESIAN_POINT('Ctrl Pts',(6.20593010073297,-4.88625474217651,8.57692807693114));
#18124=CARTESIAN_POINT('Ctrl Pts',(6.5169557998887,-4.75052124336708,8.62309627990358));
#18125=CARTESIAN_POINT('Ctrl Pts',(6.75738085499608,-4.51021173196975,8.66934525439234));
#18126=CARTESIAN_POINT('Ctrl Pts',(6.89369213325771,-4.19798398918876,8.71569439753526));
#18127=CARTESIAN_POINT('Ctrl Pts',(6.90654691277405,-3.85671872643878,8.76215710981506));
#18128=CARTESIAN_POINT('Ctrl Pts',(6.79353247440965,-3.53345392369584,8.80874771009088));
#18129=CARTESIAN_POINT('Ctrl Pts',(6.56955414486768,-3.27303442323799,8.85547967409816));
#18130=CARTESIAN_POINT('Ctrl Pts',(6.2649149706205,-3.11190453193631,8.90236637798983));
#18131=CARTESIAN_POINT('Ctrl Pts',(5.92123870946621,-3.07306727004794,8.94942058038104));
#18132=CARTESIAN_POINT('Ctrl Pts',(5.58585464057643,-3.16280189459015,8.99665488281507));
#18133=CARTESIAN_POINT('Ctrl Pts',(5.30528004465418,-3.36970780699163,9.04408084976179));
#18134=CARTESIAN_POINT('Ctrl Pts',(5.11891923625802,-3.66604749262102,9.09171075577402));
#18135=CARTESIAN_POINT('Ctrl Pts',(5.05332609200974,-4.01160086184926,9.13955361060455));
#18136=CARTESIAN_POINT('Ctrl Pts',(5.1189740076943,-4.35870259389239,9.18762398931142));
#18137=CARTESIAN_POINT('Ctrl Pts',(5.3285542005314,-4.6930196813579,9.24129614057046));
#18138=CARTESIAN_POINT('Ctrl Pts',(5.6998052948892,-4.93352876813364,9.30068292152737));
#18139=CARTESIAN_POINT('Ctrl Pts',(6.18472180410833,-4.97003234438759,9.36591862472348));
#18140=CARTESIAN_POINT('Ctrl Pts',(6.52399659312322,-4.81732094542808,9.41588571108487));
#18141=CARTESIAN_POINT('Ctrl Pts',(6.7072097546456,-4.64862385300487,9.45027233971667));
#18142=CARTESIAN_POINT('Ctrl Pts',(6.82112063385224,-4.50982226066863,9.47508293238151));
#18143=CARTESIAN_POINT('Ctrl Pts',(6.96758616721527,-4.2277942769692,9.51863575059301));
#18144=CARTESIAN_POINT('Ctrl Pts',(6.99467197393324,-3.7583480064713,9.5812519512241));
#18145=CARTESIAN_POINT('Ctrl Pts',(6.7197786782019,-3.25958856827978,9.65704089928746));
#18146=CARTESIAN_POINT('Ctrl Pts',(6.21742976902802,-2.98115434624709,9.73349110143862));
#18147=CARTESIAN_POINT('Ctrl Pts',(5.63898185512583,-3.01303591196271,9.81061012778847));
#18148=CARTESIAN_POINT('Ctrl Pts',(5.16178296910393,-3.3504033680704,9.88840029758739));
#18149=CARTESIAN_POINT('Ctrl Pts',(4.93563437526279,-3.89485977010871,9.9668597654298));
#18150=CARTESIAN_POINT('Ctrl Pts',(5.03449733338635,-4.48101061407005,10.0459867177188));
#18151=CARTESIAN_POINT('Ctrl Pts',(5.43341655784522,-4.92844358267535,10.1257712061144));
#18152=CARTESIAN_POINT('Ctrl Pts',(6.01386261401897,-5.09636465569706,10.2062013199047));
#18153=CARTESIAN_POINT('Ctrl Pts',(6.599221886597,-4.92841521164529,10.2872604826976));
#18154=CARTESIAN_POINT('Ctrl Pts',(7.00852275003305,-4.47134999264525,10.3689288213763));
#18155=CARTESIAN_POINT('Ctrl Pts',(7.11262626892049,-3.86224370688857,10.451182632454));
#18156=CARTESIAN_POINT('Ctrl Pts',(6.87506262144489,-3.28725204329248,10.5339950246611));
#18157=CARTESIAN_POINT('Ctrl Pts',(6.36475855714357,-2.92451218932454,10.6173353554807));
#18158=CARTESIAN_POINT('Ctrl Pts',(5.7359246081994,-2.88870804221006,10.7011708628368));
#18159=CARTESIAN_POINT('Ctrl Pts',(5.18151714958306,-3.19462123968635,10.785463758442));
#18160=CARTESIAN_POINT('Ctrl Pts',(4.87313525619405,-3.75143465324639,10.8701783685472));
#18161=CARTESIAN_POINT('Ctrl Pts',(4.90893297033217,-4.3896485385702,10.9552659908788));
#18162=CARTESIAN_POINT('Ctrl Pts',(5.27984440785336,-4.91323561648797,11.0406883269263));
#18163=CARTESIAN_POINT('Ctrl Pts',(5.87465010049056,-5.15984481059548,11.1263952635579));
#18164=CARTESIAN_POINT('Ctrl Pts',(6.51118263329733,-5.05207927242605,11.212352848697));
#18165=CARTESIAN_POINT('Ctrl Pts',(6.99381915840408,-4.62071977485365,11.2984788432175));
#18166=CARTESIAN_POINT('Ctrl Pts',(7.11344761293339,-4.20611912793284,11.3560318805412));
#18167=CARTESIAN_POINT('Ctrl Pts',(7.11347564185152,-3.99791344370584,11.3847750379771));
#18168=CARTESIAN_POINT('Ctrl Pts',(6.88853642595183,-4.00349313356656,2.72519438129392));
#18169=CARTESIAN_POINT('Ctrl Pts',(6.88851392453586,-3.83634677012002,2.74826922792962));
#18170=CARTESIAN_POINT('Ctrl Pts',(6.79266191595664,-3.50459201237406,2.79432671715279));
#18171=CARTESIAN_POINT('Ctrl Pts',(6.40607867092915,-3.15886656679987,2.86334141911335));
#18172=CARTESIAN_POINT('Ctrl Pts',(5.89537108171216,-3.07233178035552,2.93229916216477));
#18173=CARTESIAN_POINT('Ctrl Pts',(5.41675202428946,-3.27049076436878,3.0012653898671));
#18174=CARTESIAN_POINT('Ctrl Pts',(5.11661138750114,-3.69336572084077,3.07028597393075));
#18175=CARTESIAN_POINT('Ctrl Pts',(5.08746128376669,-4.21176251067231,3.13941287767591));
#18176=CARTESIAN_POINT('Ctrl Pts',(5.33882111712877,-4.66753429258786,3.20869886998172));
#18177=CARTESIAN_POINT('Ctrl Pts',(5.7957396457742,-4.92022616783295,3.27819757081899));
#18178=CARTESIAN_POINT('Ctrl Pts',(6.31886968522155,-4.89117427234567,3.34794867589613));
#18179=CARTESIAN_POINT('Ctrl Pts',(6.74829250702319,-4.58692636184723,3.41800335411985));
#18180=CARTESIAN_POINT('Ctrl Pts',(6.95104349855107,-4.09847642990215,3.48840505118448));
#18181=CARTESIAN_POINT('Ctrl Pts',(6.86241194209975,-3.57411489808785,3.55919775533007));
#18182=CARTESIAN_POINT('Ctrl Pts',(6.50624110521479,-3.17483224994897,3.63042194356993));
#18183=CARTESIAN_POINT('Ctrl Pts',(5.98887372723457,-3.02524962710709,3.70211601317391));
#18184=CARTESIAN_POINT('Ctrl Pts',(5.46750934114836,-3.17483111712725,3.77431546014986));
#18185=CARTESIAN_POINT('Ctrl Pts',(5.11654649260021,-3.56688533544979,3.84435869757401));
#18186=CARTESIAN_POINT('Ctrl Pts',(5.03241283783216,-3.98305413265401,3.90134876203804));
#18187=CARTESIAN_POINT('Ctrl Pts',(5.08085289836134,-4.25684105267147,3.93954512081593));
#18188=CARTESIAN_POINT('Ctrl Pts',(5.13686700531774,-4.40495648433533,3.96143070534772));
#18189=CARTESIAN_POINT('Ctrl Pts',(5.24793660806346,-4.61543096030812,3.99431888928194));
#18190=CARTESIAN_POINT('Ctrl Pts',(5.51191441648992,-4.87360832231182,4.04387894827305));
#18191=CARTESIAN_POINT('Ctrl Pts',(5.98925640546539,-5.00838455128162,4.11045355448925));
#18192=CARTESIAN_POINT('Ctrl Pts',(6.47674305919525,-4.8977142557422,4.17753674404586));
#18193=CARTESIAN_POINT('Ctrl Pts',(6.82290576508146,-4.59223022955248,4.23950296796532));
#18194=CARTESIAN_POINT('Ctrl Pts',(6.98956599692813,-4.21016952566571,4.29621883871687));
#18195=CARTESIAN_POINT('Ctrl Pts',(7.00410282218404,-3.83310156474722,4.34755879606028));
#18196=CARTESIAN_POINT('Ctrl Pts',(6.87874007455572,-3.47495996875609,4.39919719455462));
#18197=CARTESIAN_POINT('Ctrl Pts',(6.60256885276253,-3.15296728990473,4.45690377989833));
#18198=CARTESIAN_POINT('Ctrl Pts',(6.16884895912283,-2.95679731990753,4.52080650172853));
#18199=CARTESIAN_POINT('Ctrl Pts',(5.64683817264842,-2.99545349895525,4.59104572930851));
#18200=CARTESIAN_POINT('Ctrl Pts',(5.29623798334719,-3.22166642760234,4.64705739245952));
#18201=CARTESIAN_POINT('Ctrl Pts',(5.11321685115952,-3.46054845990971,4.6885396246491));
#18202=CARTESIAN_POINT('Ctrl Pts',(4.99649312835915,-3.69129778885919,4.72419099996777));
#18203=CARTESIAN_POINT('Ctrl Pts',(4.93515842947507,-4.01438075257337,4.76893235210618));
#18204=CARTESIAN_POINT('Ctrl Pts',(5.00884138794006,-4.40411676050145,4.82290104831588));
#18205=CARTESIAN_POINT('Ctrl Pts',(5.22069691149792,-4.74188211024749,4.87714211347641));
#18206=CARTESIAN_POINT('Ctrl Pts',(5.54294475281331,-4.979743888843,4.93165037763781));
#18207=CARTESIAN_POINT('Ctrl Pts',(5.93184914211983,-5.08439121416751,4.98641884848078));
#18208=CARTESIAN_POINT('Ctrl Pts',(6.33337868619195,-5.03891906119859,5.04143962102492));
#18209=CARTESIAN_POINT('Ctrl Pts',(6.81344622817293,-4.78714604268289,5.11512659410201));
#18210=CARTESIAN_POINT('Ctrl Pts',(7.17386284388877,-4.16740765547856,5.20781208817404));
#18211=CARTESIAN_POINT('Ctrl Pts',(6.98151177291868,-3.31910065636828,5.31989742715281));
#18212=CARTESIAN_POINT('Ctrl Pts',(6.38018037258757,-2.90949829895718,5.41393652817617));
#18213=CARTESIAN_POINT('Ctrl Pts',(5.82452419881361,-2.89038561056404,5.4895085736308));
#18214=CARTESIAN_POINT('Ctrl Pts',(5.38643937700961,-3.0426430278763,5.55265631890358));
#18215=CARTESIAN_POINT('Ctrl Pts',(5.0145022718477,-3.40495936093987,5.62231958033395));
#18216=CARTESIAN_POINT('Ctrl Pts',(4.84717711780572,-3.94776217453295,5.69853006603046));
#18217=CARTESIAN_POINT('Ctrl Pts',(4.94099186919954,-4.41256002942381,5.76219880693713));
#18218=CARTESIAN_POINT('Ctrl Pts',(5.11766856031632,-4.68536215086932,5.80682961590476));
#18219=CARTESIAN_POINT('Ctrl Pts',(5.24493119859604,-4.81913238240527,5.83235224216694));
#18220=CARTESIAN_POINT('Ctrl Pts',(5.45930477431542,-4.9948414663518,5.87065055301519));
#18221=CARTESIAN_POINT('Ctrl Pts',(5.85797322925551,-5.15141705336824,5.92814987557556));
#18222=CARTESIAN_POINT('Ctrl Pts',(6.37807174974638,-5.08631909572604,5.99849836625092));
#18223=CARTESIAN_POINT('Ctrl Pts',(6.77618145548473,-4.83577308391186,6.06247866417908));
#18224=CARTESIAN_POINT('Ctrl Pts',(7.02758555630676,-4.49525125160203,6.12008054118587));
#18225=CARTESIAN_POINT('Ctrl Pts',(7.13717722861579,-4.08632109309765,6.1776704930539));
#18226=CARTESIAN_POINT('Ctrl Pts',(7.08979000943633,-3.66582201155788,6.23524265529162));
#18227=CARTESIAN_POINT('Ctrl Pts',(6.89204673042122,-3.29205056628206,6.29277697865426));
#18228=CARTESIAN_POINT('Ctrl Pts',(6.5718504683246,-3.01633590404546,6.35026012152877));
#18229=CARTESIAN_POINT('Ctrl Pts',(6.17349702418284,-2.87727195418905,6.40767537367819));
#18230=CARTESIAN_POINT('Ctrl Pts',(5.68208662701439,-2.89527617243405,6.47456940039547));
#18231=CARTESIAN_POINT('Ctrl Pts',(5.18032599444233,-3.17179956913016,6.55085081859633));
#18232=CARTESIAN_POINT('Ctrl Pts',(4.86989550108574,-3.73521723461931,6.63640620982512));
#18233=CARTESIAN_POINT('Ctrl Pts',(4.90018724897131,-4.26763558163364,6.70744811984369));
#18234=CARTESIAN_POINT('Ctrl Pts',(5.09065881531276,-4.6346219832112,6.76410197014731));
#18235=CARTESIAN_POINT('Ctrl Pts',(5.32642853144266,-4.88432892504754,6.81120999936015));
#18236=CARTESIAN_POINT('Ctrl Pts',(5.66244422861094,-5.06182402697993,6.86288433937329));
#18237=CARTESIAN_POINT('Ctrl Pts',(6.07263963889414,-5.10781715858294,6.91907132462124));
#18238=CARTESIAN_POINT('Ctrl Pts',(6.53667667508948,-4.98388363300407,6.98438658115342));
#18239=CARTESIAN_POINT('Ctrl Pts',(6.95258347663703,-4.61205745986084,7.05868174802314));
#18240=CARTESIAN_POINT('Ctrl Pts',(7.12466537226074,-4.01175995341158,7.14174808909433));
#18241=CARTESIAN_POINT('Ctrl Pts',(6.95256249513245,-3.41639873131959,7.22427322871735));
#18242=CARTESIAN_POINT('Ctrl Pts',(6.49303513416945,-3.00635077992184,7.30622569076459));
#18243=CARTESIAN_POINT('Ctrl Pts',(5.89035880333171,-2.90495807984544,7.38758293290033));
#18244=CARTESIAN_POINT('Ctrl Pts',(5.33018372919521,-3.13754016396607,7.46832214054757));
#18245=CARTESIAN_POINT('Ctrl Pts',(4.98265794015465,-3.62878963133895,7.54842402890944));
#18246=CARTESIAN_POINT('Ctrl Pts',(4.94959218817397,-4.22473472744915,7.62787515983858));
#18247=CARTESIAN_POINT('Ctrl Pts',(5.23670236553316,-4.74246459176775,7.7066648962458));
#18248=CARTESIAN_POINT('Ctrl Pts',(5.75070331377736,-5.02573461363327,7.78478658453007));
#18249=CARTESIAN_POINT('Ctrl Pts',(6.3315944612577,-4.99238023588094,7.86223715968712));
#18250=CARTESIAN_POINT('Ctrl Pts',(6.80176712773346,-4.65807183999786,7.93901966146638));
#18251=CARTESIAN_POINT('Ctrl Pts',(7.01966294687514,-4.12940487515114,8.01513582983289));
#18252=CARTESIAN_POINT('Ctrl Pts',(6.92418292551131,-3.57072879727912,8.09059580794518));
#18253=CARTESIAN_POINT('Ctrl Pts',(6.54906751855537,-3.15201220927634,8.16541569688595));
#18254=CARTESIAN_POINT('Ctrl Pts',(6.01345996886975,-2.99852359627092,8.23960831004383));
#18255=CARTESIAN_POINT('Ctrl Pts',(5.48217439877857,-3.15184573564912,8.31320179685831));
#18256=CARTESIAN_POINT('Ctrl Pts',(5.13089843772479,-3.54612521955196,8.38350581076996));
#18257=CARTESIAN_POINT('Ctrl Pts',(5.0326487563089,-4.0364884839662,8.45062953683967));
#18258=CARTESIAN_POINT('Ctrl Pts',(5.17319067664245,-4.49223316217463,8.51464838787996));
#18259=CARTESIAN_POINT('Ctrl Pts',(5.48463728440744,-4.79523144276229,8.5729734529706));
#18260=CARTESIAN_POINT('Ctrl Pts',(5.85075368554384,-4.92293243199514,8.62572747369152));
#18261=CARTESIAN_POINT('Ctrl Pts',(6.19801348687623,-4.90991155246289,8.67301780183671));
#18262=CARTESIAN_POINT('Ctrl Pts',(6.51522255886468,-4.77128712747284,8.72011840453903));
#18263=CARTESIAN_POINT('Ctrl Pts',(6.75903612701758,-4.52733816748863,8.76705321549295));
#18264=CARTESIAN_POINT('Ctrl Pts',(6.89641433024893,-4.21221927191064,8.81382959040646));
#18265=CARTESIAN_POINT('Ctrl Pts',(6.90913619885495,-3.86977043889933,8.86046173222151));
#18266=CARTESIAN_POINT('Ctrl Pts',(6.79619374111234,-3.54724787641334,8.90696283891172));
#18267=CARTESIAN_POINT('Ctrl Pts',(6.57379330446791,-3.28893297442313,8.95334702636426));
#18268=CARTESIAN_POINT('Ctrl Pts',(6.27306517518208,-3.13006968654134,8.99962841810225));
#18269=CARTESIAN_POINT('Ctrl Pts',(5.93572658739197,-3.0921235656841,9.0458216557526));
#18270=CARTESIAN_POINT('Ctrl Pts',(5.60836618975707,-3.17988842208988,9.09194124619793));
#18271=CARTESIAN_POINT('Ctrl Pts',(5.33602236999747,-3.38093608109373,9.13800263745416));
#18272=CARTESIAN_POINT('Ctrl Pts',(5.15614240909104,-3.66727534380435,9.18401982014308));
#18273=CARTESIAN_POINT('Ctrl Pts',(5.09326323380394,-3.99940669517924,9.23001051026176));
#18274=CARTESIAN_POINT('Ctrl Pts',(5.15618727724121,-4.33129335464849,9.27598439739637));
#18275=CARTESIAN_POINT('Ctrl Pts',(5.35578605418237,-4.64936719014534,9.32706877285428));
#18276=CARTESIAN_POINT('Ctrl Pts',(5.70736198634476,-4.87675366561928,9.3832866314104));
#18277=CARTESIAN_POINT('Ctrl Pts',(6.16369266354364,-4.91077958536555,9.44468658180074));
#18278=CARTESIAN_POINT('Ctrl Pts',(6.48109710311922,-4.76766612382848,9.49145069598086));
#18279=CARTESIAN_POINT('Ctrl Pts',(6.65197106906924,-4.61031651982011,9.52352657457864));
#18280=CARTESIAN_POINT('Ctrl Pts',(6.75806246750007,-4.48103427992951,9.54663607519105));
#18281=CARTESIAN_POINT('Ctrl Pts',(6.89415792745756,-4.21884193757629,9.58712522676296));
#18282=CARTESIAN_POINT('Ctrl Pts',(6.91894087007071,-3.78418172620761,9.64510513260814));
#18283=CARTESIAN_POINT('Ctrl Pts',(6.66534324481484,-3.32472290943998,9.71495345065709));
#18284=CARTESIAN_POINT('Ctrl Pts',(6.20419942989133,-3.06944166542164,9.78511977938196));
#18285=CARTESIAN_POINT('Ctrl Pts',(5.67524333022435,-3.09882568028089,9.85564775939405));
#18286=CARTESIAN_POINT('Ctrl Pts',(5.24024568965602,-3.40659380896812,9.92658189146111));
#18287=CARTESIAN_POINT('Ctrl Pts',(5.03464763548414,-3.90193118025057,9.99796464537582));
#18288=CARTESIAN_POINT('Ctrl Pts',(5.12452333571866,-4.43421378319489,10.0698272337774));
#18289=CARTESIAN_POINT('Ctrl Pts',(5.48642962474464,-4.84005659450095,10.1422070537588));
#18290=CARTESIAN_POINT('Ctrl Pts',(6.01270459980476,-4.99229906382123,10.2151342966527));
#18291=CARTESIAN_POINT('Ctrl Pts',(6.54349151359531,-4.84004652702854,10.2886377190555));
#18292=CARTESIAN_POINT('Ctrl Pts',(6.91493654437396,-4.42537746826921,10.3627418267029));
#18293=CARTESIAN_POINT('Ctrl Pts',(7.00963644867476,-3.87203813765055,10.4374679148733));
#18294=CARTESIAN_POINT('Ctrl Pts',(6.79358830396164,-3.34867882889457,10.5128334140703));
#18295=CARTESIAN_POINT('Ctrl Pts',(6.32822477073631,-3.01762364049853,10.5888520780036));
#18296=CARTESIAN_POINT('Ctrl Pts',(5.75303331970575,-2.98461572568303,10.665533657142));
#18297=CARTESIAN_POINT('Ctrl Pts',(5.24411579401217,-3.26509167414394,10.7428842026003));
#18298=CARTESIAN_POINT('Ctrl Pts',(4.95977091463743,-3.77778621479579,10.8209053147198));
#18299=CARTESIAN_POINT('Ctrl Pts',(4.99250844096273,-4.36807972196266,10.8995957097798));
#18300=CARTESIAN_POINT('Ctrl Pts',(5.33676307768738,-4.85473515789548,10.9789525208368));
#18301=CARTESIAN_POINT('Ctrl Pts',(5.89185847419169,-5.0853624635031,11.0589565134979));
#18302=CARTESIAN_POINT('Ctrl Pts',(6.48921656678778,-4.98467525931286,11.1396133726823));
#18303=CARTESIAN_POINT('Ctrl Pts',(6.94489938062386,-4.57808986983126,11.2208627112899));
#18304=CARTESIAN_POINT('Ctrl Pts',(7.05869952443909,-4.18467099703403,11.2754820789842));
#18305=CARTESIAN_POINT('Ctrl Pts',(7.05872618995271,-3.98659301618569,11.3028270893246));
#18306=CARTESIAN_POINT('Ctrl Pts',(6.95029270794106,-4.01413412167565,2.80233431196407));
#18307=CARTESIAN_POINT('Ctrl Pts',(6.95026870797549,-3.83585614248054,2.82694589754466));
#18308=CARTESIAN_POINT('Ctrl Pts',(6.84793152004367,-3.48237875324069,2.87602065146748));
#18309=CARTESIAN_POINT('Ctrl Pts',(6.43858029515218,-3.11708365014168,2.94901647539155));
#18310=CARTESIAN_POINT('Ctrl Pts',(5.90189353794577,-3.02662837560554,3.02147175614449));
#18311=CARTESIAN_POINT('Ctrl Pts',(5.40287867078653,-3.23386954835159,3.09339843495734));
#18312=CARTESIAN_POINT('Ctrl Pts',(5.09267659494215,-3.67194351384352,3.16483831483556));
#18313=CARTESIAN_POINT('Ctrl Pts',(5.06334698391922,-4.20438701666129,3.23582633137519));
#18314=CARTESIAN_POINT('Ctrl Pts',(5.31996060248519,-4.66840757573284,3.30640065967282));
#18315=CARTESIAN_POINT('Ctrl Pts',(5.78190061537116,-4.92314894439882,3.37659959628945));
#18316=CARTESIAN_POINT('Ctrl Pts',(6.30602360446337,-4.8934194778442,3.44647512179493));
#18317=CARTESIAN_POINT('Ctrl Pts',(6.73235320697049,-4.59059886848916,3.51606957003369));
#18318=CARTESIAN_POINT('Ctrl Pts',(6.93158527369931,-4.10903724627938,3.58543222201393));
#18319=CARTESIAN_POINT('Ctrl Pts',(6.84437087172348,-3.5966316690937,3.65461147199652));
#18320=CARTESIAN_POINT('Ctrl Pts',(6.4986005712581,-3.20987659405636,3.72365772216215));
#18321=CARTESIAN_POINT('Ctrl Pts',(6.00069620889802,-3.06649917569834,3.79262193940454));
#18322=CARTESIAN_POINT('Ctrl Pts',(5.50298206081782,-3.20985050236122,3.86155519007754));
#18323=CARTESIAN_POINT('Ctrl Pts',(5.17058746032825,-3.58189591316552,3.9279559301895));
#18324=CARTESIAN_POINT('Ctrl Pts',(5.09161084911067,-3.97403244462459,3.98163982698735));
#18325=CARTESIAN_POINT('Ctrl Pts',(5.13710290917312,-4.23088993114173,4.01747369242388));
#18326=CARTESIAN_POINT('Ctrl Pts',(5.18955604905821,-4.36957304831134,4.03796514432227));
#18327=CARTESIAN_POINT('Ctrl Pts',(5.29342590228157,-4.56638378889049,4.06871725914488));
#18328=CARTESIAN_POINT('Ctrl Pts',(5.53958614449405,-4.80683581259022,4.11489405980733));
#18329=CARTESIAN_POINT('Ctrl Pts',(5.98240799870313,-4.93159290708471,4.17664221174671));
#18330=CARTESIAN_POINT('Ctrl Pts',(6.43251496390311,-4.82915258042553,4.23858449276294));
#18331=CARTESIAN_POINT('Ctrl Pts',(6.75076512217874,-4.54803787118636,4.29557302280714));
#18332=CARTESIAN_POINT('Ctrl Pts',(6.90350439608594,-4.1976580738955,4.34757883005092));
#18333=CARTESIAN_POINT('Ctrl Pts',(6.91672786492714,-3.85270518195888,4.39454228245137));
#18334=CARTESIAN_POINT('Ctrl Pts',(6.80221870211402,-3.52577730207959,4.44168103975221));
#18335=CARTESIAN_POINT('Ctrl Pts',(6.55050308426461,-3.23240263631744,4.4942637068826));
#18336=CARTESIAN_POINT('Ctrl Pts',(6.1559407673884,-3.05405612320139,4.55238887331135));
#18337=CARTESIAN_POINT('Ctrl Pts',(5.68186673349783,-3.08924643489957,4.61617826163733));
#18338=CARTESIAN_POINT('Ctrl Pts',(5.36384514849828,-3.29450208863786,4.66698585997441));
#18339=CARTESIAN_POINT('Ctrl Pts',(5.19788403496136,-3.51112297261418,4.704601695143));
#18340=CARTESIAN_POINT('Ctrl Pts',(5.09206016360501,-3.72033550049983,4.73692459134345));
#18341=CARTESIAN_POINT('Ctrl Pts',(5.03646402164839,-4.01321713560672,4.77748324312575));
#18342=CARTESIAN_POINT('Ctrl Pts',(5.10326084825423,-4.36654385903782,4.82640948098865));
#18343=CARTESIAN_POINT('Ctrl Pts',(5.29537719841234,-4.67285861362723,4.87559956298535));
#18344=CARTESIAN_POINT('Ctrl Pts',(5.58777289090629,-4.88870901734329,4.92506008683499));
#18345=CARTESIAN_POINT('Ctrl Pts',(5.94094293939234,-4.98377199421309,4.97479853966587));
#18346=CARTESIAN_POINT('Ctrl Pts',(6.30598645054714,-4.94246709481662,5.0248192914387));
#18347=CARTESIAN_POINT('Ctrl Pts',(6.74299909696092,-4.71334423715881,5.0918971423708));
#18348=CARTESIAN_POINT('Ctrl Pts',(7.07217428481599,-4.14811709402513,5.17646845460267));
#18349=CARTESIAN_POINT('Ctrl Pts',(6.89663854890958,-3.37095216653505,5.27914241536394));
#18350=CARTESIAN_POINT('Ctrl Pts',(6.34353600825991,-2.99345577262945,5.36570002215199));
#18351=CARTESIAN_POINT('Ctrl Pts',(5.83000485848951,-2.97563765967302,5.43554273377057));
#18352=CARTESIAN_POINT('Ctrl Pts',(5.42395250164482,-3.11665383947864,5.49407446014151));
#18353=CARTESIAN_POINT('Ctrl Pts',(5.07781352815922,-3.45348334377841,5.55887851989237));
#18354=CARTESIAN_POINT('Ctrl Pts',(4.92119569589212,-3.96053443240852,5.63008962860051));
#18355=CARTESIAN_POINT('Ctrl Pts',(5.00900201580092,-4.39683944226663,5.68985207204882));
#18356=CARTESIAN_POINT('Ctrl Pts',(5.17540309970581,-4.65387162944169,5.7319018911364));
#18357=CARTESIAN_POINT('Ctrl Pts',(5.29550761861826,-4.78012386768163,5.75599031365937));
#18358=CARTESIAN_POINT('Ctrl Pts',(5.49807304938454,-4.94616553552845,5.79218348973528));
#18359=CARTESIAN_POINT('Ctrl Pts',(5.87591495189871,-5.09483660418974,5.84669780842769));
#18360=CARTESIAN_POINT('Ctrl Pts',(6.37161693207542,-5.03311956022957,5.91374966034583));
#18361=CARTESIAN_POINT('Ctrl Pts',(6.75295541512623,-4.79334050443991,5.97502993095026));
#18362=CARTESIAN_POINT('Ctrl Pts',(6.9948086761482,-4.46601711692582,6.03041678164421));
#18363=CARTESIAN_POINT('Ctrl Pts',(7.10079809559249,-4.07117534641981,6.08603676959893));
#18364=CARTESIAN_POINT('Ctrl Pts',(7.0550052284071,-3.66335712376636,6.14187488824605));
#18365=CARTESIAN_POINT('Ctrl Pts',(6.86254272821113,-3.29919610730441,6.19792289616172));
#18366=CARTESIAN_POINT('Ctrl Pts',(6.54938376947623,-3.02931907732678,6.25416911836834));
#18367=CARTESIAN_POINT('Ctrl Pts',(6.1579486558425,-2.89248546959741,6.31060244716706));
#18368=CARTESIAN_POINT('Ctrl Pts',(5.67285796098016,-2.91005237096891,6.37664094306513));
#18369=CARTESIAN_POINT('Ctrl Pts',(5.17447535525086,-3.18410669330449,6.4523908315935));
#18370=CARTESIAN_POINT('Ctrl Pts',(4.86359518381245,-3.74699626482779,6.53792551889047));
#18371=CARTESIAN_POINT('Ctrl Pts',(4.89358978229736,-4.28284509764931,6.60942647452156));
#18372=CARTESIAN_POINT('Ctrl Pts',(5.08616754915788,-4.65413963922357,6.66674144768274));
#18373=CARTESIAN_POINT('Ctrl Pts',(5.32539997681471,-4.90762443384318,6.71455792748918));
#18374=CARTESIAN_POINT('Ctrl Pts',(5.66770904279484,-5.08864325266815,6.76722197047057));
#18375=CARTESIAN_POINT('Ctrl Pts',(6.08751475108002,-5.13588298949551,6.82473049674227));
#18376=CARTESIAN_POINT('Ctrl Pts',(6.5645861835624,-5.00869269277779,6.891883208414));
#18377=CARTESIAN_POINT('Ctrl Pts',(6.99480434755378,-4.62476574907813,6.96867942951375));
#18378=CARTESIAN_POINT('Ctrl Pts',(7.17439385392664,-4.000445623383,7.05510766898402));
#18379=CARTESIAN_POINT('Ctrl Pts',(6.99478104501133,-3.37709835463719,7.14150114377049));
#18380=CARTESIAN_POINT('Ctrl Pts',(6.51124152718936,-2.94487966771886,7.2278171181847));
#18381=CARTESIAN_POINT('Ctrl Pts',(5.87300157020658,-2.83697217244672,7.31399284682077));
#18382=CARTESIAN_POINT('Ctrl Pts',(5.27624103646301,-3.08421455661578,7.39998347287708));
#18383=CARTESIAN_POINT('Ctrl Pts',(4.90381274036846,-3.60985955031299,7.48574172113935));
#18384=CARTESIAN_POINT('Ctrl Pts',(4.86781101481599,-4.25096067395124,7.57122146774242));
#18385=CARTESIAN_POINT('Ctrl Pts',(5.17774894918109,-4.81069654524739,7.6563808117967));
#18386=CARTESIAN_POINT('Ctrl Pts',(5.73539207552131,-5.11843269669984,7.74116666788786));
#18387=CARTESIAN_POINT('Ctrl Pts',(6.36818899742731,-5.08242658049411,7.82554016071411));
#18388=CARTESIAN_POINT('Ctrl Pts',(6.88223000977129,-4.71728080679399,7.90946350349862));
#18389=CARTESIAN_POINT('Ctrl Pts',(7.12127708571697,-4.13791637661882,7.9928932228046));
#18390=CARTESIAN_POINT('Ctrl Pts',(7.01656472861822,-3.52409769071585,8.07579754700462));
#18391=CARTESIAN_POINT('Ctrl Pts',(6.60378953069044,-3.0631252600952,8.15814989617874));
#18392=CARTESIAN_POINT('Ctrl Pts',(6.01351012908046,-2.89387326118091,8.23991854958376));
#18393=CARTESIAN_POINT('Ctrl Pts',(5.42751466531372,-3.06292659016434,8.32108499418846));
#18394=CARTESIAN_POINT('Ctrl Pts',(5.04001126571795,-3.49787745920239,8.39863860309313));
#18395=CARTESIAN_POINT('Ctrl Pts',(4.93170509712578,-4.03860077006941,8.47265039810351));
#18396=CARTESIAN_POINT('Ctrl Pts',(5.0866102730624,-4.5407113707165,8.54318119360061));
#18397=CARTESIAN_POINT('Ctrl Pts',(5.42936100250732,-4.87403779849933,8.60735376890046));
#18398=CARTESIAN_POINT('Ctrl Pts',(5.83158616216201,-5.01427171038084,8.66530592755971));
#18399=CARTESIAN_POINT('Ctrl Pts',(6.21244337123709,-4.9999360439205,8.71716546435109));
#18400=CARTESIAN_POINT('Ctrl Pts',(6.5596673206854,-4.84811610405237,8.76872530395661));
#18401=CARTESIAN_POINT('Ctrl Pts',(6.82593444340501,-4.58159404350882,8.81998719323947));
#18402=CARTESIAN_POINT('Ctrl Pts',(6.97555097229746,-4.23818719630342,8.87095217885581));
#18403=CARTESIAN_POINT('Ctrl Pts',(6.98928103115449,-3.86603752953955,8.92162246922555));
#18404=CARTESIAN_POINT('Ctrl Pts',(6.86680877161237,-3.51661440857094,8.97200097582266));
#18405=CARTESIAN_POINT('Ctrl Pts',(6.62652276655028,-3.23769642671214,9.02209139324216));
#18406=CARTESIAN_POINT('Ctrl Pts',(6.30278853986408,-3.066814257131,9.07189819214372));
#18407=CARTESIAN_POINT('Ctrl Pts',(5.94102919446653,-3.02624740788871,9.12142652419554));
#18408=CARTESIAN_POINT('Ctrl Pts',(5.59139099220371,-3.12012203285758,9.17068242089275));
#18409=CARTESIAN_POINT('Ctrl Pts',(5.30176852740219,-3.33409677722697,9.21967228892019));
#18410=CARTESIAN_POINT('Ctrl Pts',(5.11137229937622,-3.6374484355137,9.26840399241005));
#18411=CARTESIAN_POINT('Ctrl Pts',(5.04522577317681,-3.98765556961418,9.31688436084706));
#18412=CARTESIAN_POINT('Ctrl Pts',(5.11140993276018,-4.3359118298156,9.36512475134174));
#18413=CARTESIAN_POINT('Ctrl Pts',(5.32001499181377,-4.66799152448505,9.41846713475402));
#18414=CARTESIAN_POINT('Ctrl Pts',(5.68522837066175,-4.90377380153277,9.47682628398783));
#18415=CARTESIAN_POINT('Ctrl Pts',(6.15572665009444,-4.93842778603278,9.54011788753042));
#18416=CARTESIAN_POINT('Ctrl Pts',(6.48054112448135,-4.79164030355885,9.58798704654535));
#18417=CARTESIAN_POINT('Ctrl Pts',(6.65464130933801,-4.63128846987969,9.62066963734384));
#18418=CARTESIAN_POINT('Ctrl Pts',(6.76252419033915,-4.49981139232218,9.64416932945342));
#18419=CARTESIAN_POINT('Ctrl Pts',(6.90041745117454,-4.23395162044738,9.68520793907203));
#18420=CARTESIAN_POINT('Ctrl Pts',(6.92488338590534,-3.79600782000729,9.7436137313988));
#18421=CARTESIAN_POINT('Ctrl Pts',(6.67096107275452,-3.33726536059452,9.81338971644578));
#18422=CARTESIAN_POINT('Ctrl Pts',(6.2137581090805,-3.08487281006037,9.88290182303105));
#18423=CARTESIAN_POINT('Ctrl Pts',(5.69400607020532,-3.11435421989238,9.95220006390264));
#18424=CARTESIAN_POINT('Ctrl Pts',(5.27034711588601,-3.41482578093218,10.0213303098789));
#18425=CARTESIAN_POINT('Ctrl Pts',(5.0720867380328,-3.89402097251012,10.0903392614919));
#18426=CARTESIAN_POINT('Ctrl Pts',(5.15887741676057,-4.40470662845712,10.1592876980663));
#18427=CARTESIAN_POINT('Ctrl Pts',(5.50401868453627,-4.79094481054898,10.228222582476));
#18428=CARTESIAN_POINT('Ctrl Pts',(6.00198308450928,-4.93447537956818,10.297197459271));
#18429=CARTESIAN_POINT('Ctrl Pts',(6.50066246085064,-4.79094442895005,10.3662628212364));
#18430=CARTESIAN_POINT('Ctrl Pts',(6.8472808539946,-4.4033400083843,10.4354699282555));
#18431=CARTESIAN_POINT('Ctrl Pts',(6.93484780248239,-3.88932387200705,10.5048686867946));
#18432=CARTESIAN_POINT('Ctrl Pts',(6.73486307134074,-3.40581622442059,10.5745079681309));
#18433=CARTESIAN_POINT('Ctrl Pts',(6.30656413212906,-3.10151906733419,10.6444355131787));
#18434=CARTESIAN_POINT('Ctrl Pts',(5.77947299474872,-3.07154831166864,10.714696453497));
#18435=CARTESIAN_POINT('Ctrl Pts',(5.31478999974729,-3.32791188545808,10.785335947611));
#18436=CARTESIAN_POINT('Ctrl Pts',(5.05597365417069,-3.79497493605006,10.8563922532882));
#18437=CARTESIAN_POINT('Ctrl Pts',(5.08587069642077,-4.3314820844115,10.9279113545464));
#18438=CARTESIAN_POINT('Ctrl Pts',(5.39837456971601,-4.77309564174969,10.9999287051914));
#18439=CARTESIAN_POINT('Ctrl Pts',(5.90171757367533,-4.98215829124314,11.0724701515572));
#18440=CARTESIAN_POINT('Ctrl Pts',(6.4432028732693,-4.89091322567894,11.1455775949948));
#18441=CARTESIAN_POINT('Ctrl Pts',(6.85641784710808,-4.52222909517366,11.2192551426726));
#18442=CARTESIAN_POINT('Ctrl Pts',(6.95974791691079,-4.16531628624991,11.2688068655971));
#18443=CARTESIAN_POINT('Ctrl Pts',(6.95977214909355,-3.98531368433122,11.2936565383859));
#18444=CARTESIAN_POINT('Ctrl Pts',(7.04959557699666,-4.01407739529388,2.80202024039622));
#18445=CARTESIAN_POINT('Ctrl Pts',(7.04956913822907,-3.81768336112141,2.82913277892384));
#18446=CARTESIAN_POINT('Ctrl Pts',(6.9367202622634,-3.42769410118136,2.88327931957377));
#18447=CARTESIAN_POINT('Ctrl Pts',(6.48516094749322,-3.0248175347279,2.96379344062057));
#18448=CARTESIAN_POINT('Ctrl Pts',(5.89336937954221,-2.92510533993989,3.04369509984053));
#18449=CARTESIAN_POINT('Ctrl Pts',(5.34372152306085,-3.15350875728527,3.12292785038527));
#18450=CARTESIAN_POINT('Ctrl Pts',(5.00270118788897,-3.63538461147314,3.20150168364572));
#18451=CARTESIAN_POINT('Ctrl Pts',(4.9707269774799,-4.2196676866048,3.2794028151618));
#18452=CARTESIAN_POINT('Ctrl Pts',(5.25175807656894,-4.72729550009722,3.35663469084281));
#18453=CARTESIAN_POINT('Ctrl Pts',(5.75566327080534,-5.00482201266583,3.43319899049717));
#18454=CARTESIAN_POINT('Ctrl Pts',(6.32490283312075,-4.97217868326178,3.50910125356791));
#18455=CARTESIAN_POINT('Ctrl Pts',(6.78559126572007,-4.64446921311548,3.58435264375379));
#18456=CARTESIAN_POINT('Ctrl Pts',(6.99947417356179,-4.12635582910261,3.65896738189));
#18457=CARTESIAN_POINT('Ctrl Pts',(6.90573630851746,-3.57844037550777,3.73296376784759));
#18458=CARTESIAN_POINT('Ctrl Pts',(6.53785050039439,-3.16771161668764,3.80636369579688));
#18459=CARTESIAN_POINT('Ctrl Pts',(6.01199576895297,-3.01684493282177,3.87919245676609));
#18460=CARTESIAN_POINT('Ctrl Pts',(5.49033214833547,-3.16768487910272,3.95147922807082));
#18461=CARTESIAN_POINT('Ctrl Pts',(5.14483056253905,-3.55524231144764,4.02059698653933));
#18462=CARTESIAN_POINT('Ctrl Pts',(5.0635938893428,-3.96044031254016,4.07607444285223));
#18463=CARTESIAN_POINT('Ctrl Pts',(5.1104030580457,-4.22437750124471,4.11290332834221));
#18464=CARTESIAN_POINT('Ctrl Pts',(5.16416796568317,-4.36650518820908,4.13390550744089));
#18465=CARTESIAN_POINT('Ctrl Pts',(5.27044638425171,-4.56784578375605,4.16536782181109));
#18466=CARTESIAN_POINT('Ctrl Pts',(5.52142748309971,-4.81253448522336,4.21242232862903));
#18467=CARTESIAN_POINT('Ctrl Pts',(5.96924076086895,-4.9382410071469,4.27485485012556));
#18468=CARTESIAN_POINT('Ctrl Pts',(6.42087513852533,-4.83500709645662,4.3370303440752));
#18469=CARTESIAN_POINT('Ctrl Pts',(6.73765110446275,-4.55466041922396,4.39381972192088));
#18470=CARTESIAN_POINT('Ctrl Pts',(6.88864417341743,-4.20781172341044,4.44529669035746));
#18471=CARTESIAN_POINT('Ctrl Pts',(6.90147923264546,-3.86824513057332,4.49153432087195));
#18472=CARTESIAN_POINT('Ctrl Pts',(6.78923182972319,-3.54825327547411,4.53768901187963));
#18473=CARTESIAN_POINT('Ctrl Pts',(6.54396727764667,-3.26270069623157,4.58889957043465));
#18474=CARTESIAN_POINT('Ctrl Pts',(6.16200255235145,-3.09043995215812,4.64515540035398));
#18475=CARTESIAN_POINT('Ctrl Pts',(5.70640445778069,-3.12464870133968,4.70646763990055));
#18476=CARTESIAN_POINT('Ctrl Pts',(5.40286749556076,-3.32088745545974,4.75500864335017));
#18477=CARTESIAN_POINT('Ctrl Pts',(5.24512838139169,-3.5268208069634,4.79077034626969));
#18478=CARTESIAN_POINT('Ctrl Pts',(5.14477881719594,-3.72525665024375,4.82142974515389));
#18479=CARTESIAN_POINT('Ctrl Pts',(5.09234818824701,-4.00210562688859,4.85977002075827));
#18480=CARTESIAN_POINT('Ctrl Pts',(5.15533182225625,-4.33458130178686,4.90581914691398));
#18481=CARTESIAN_POINT('Ctrl Pts',(5.33548776796468,-4.6215748362361,4.95192433144584));
#18482=CARTESIAN_POINT('Ctrl Pts',(5.60848260587076,-4.82296944796147,4.99809986716363));
#18483=CARTESIAN_POINT('Ctrl Pts',(5.9369440104669,-4.91125654772996,5.04435881769998));
#18484=CARTESIAN_POINT('Ctrl Pts',(6.27520360585225,-4.87289052404234,5.0907169889183));
#18485=CARTESIAN_POINT('Ctrl Pts',(6.6787996200642,-4.66111658918346,5.15267727991992));
#18486=CARTESIAN_POINT('Ctrl Pts',(6.98098150122638,-4.14106395747072,5.23045754094985));
#18487=CARTESIAN_POINT('Ctrl Pts',(6.81977626230843,-3.43017766460645,5.32440599363029));
#18488=CARTESIAN_POINT('Ctrl Pts',(6.31552816547733,-3.08645665568759,5.40330039236375));
#18489=CARTESIAN_POINT('Ctrl Pts',(5.84855411100682,-3.07029855427464,5.46681774835805));
#18490=CARTESIAN_POINT('Ctrl Pts',(5.4797268769858,-3.19842337273609,5.51998686657359));
#18491=CARTESIAN_POINT('Ctrl Pts',(5.16567222350704,-3.50409863861733,5.57879374554913));
#18492=CARTESIAN_POINT('Ctrl Pts',(5.02366796970531,-3.96389006248025,5.64337126252039));
#18493=CARTESIAN_POINT('Ctrl Pts',(5.1032679493576,-4.35943860083833,5.69755174644111));
#18494=CARTESIAN_POINT('Ctrl Pts',(5.25414338424139,-4.59250987985455,5.7356818133743));
#18495=CARTESIAN_POINT('Ctrl Pts',(5.3630668329631,-4.70701089826391,5.75752797728752));
#18496=CARTESIAN_POINT('Ctrl Pts',(5.54680053310836,-4.85761941833764,5.79035698196648));
#18497=CARTESIAN_POINT('Ctrl Pts',(5.88965278851035,-4.9925747646598,5.83982581730757));
#18498=CARTESIAN_POINT('Ctrl Pts',(6.33999449822917,-4.93659055838853,5.90073991716705));
#18499=CARTESIAN_POINT('Ctrl Pts',(6.6869391381759,-4.71851451977266,5.95648601990599));
#18500=CARTESIAN_POINT('Ctrl Pts',(6.90731245937833,-4.42035144578017,6.00694356452062));
#18501=CARTESIAN_POINT('Ctrl Pts',(7.00409117035043,-4.06008469798609,6.05769403505103));
#18502=CARTESIAN_POINT('Ctrl Pts',(6.96230174690874,-3.68725672811026,6.10873851183451));
#18503=CARTESIAN_POINT('Ctrl Pts',(6.78606403741209,-3.35362517017195,6.16007991043999));
#18504=CARTESIAN_POINT('Ctrl Pts',(6.49860389913839,-3.10577421388223,6.21171855444694));
#18505=CARTESIAN_POINT('Ctrl Pts',(6.13835846199652,-2.97974364176408,6.26365546641588));
#18506=CARTESIAN_POINT('Ctrl Pts',(5.69070282319273,-2.99583565516249,6.32459628110795));
#18507=CARTESIAN_POINT('Ctrl Pts',(5.22903186486354,-3.24932298263957,6.39473487294707));
#18508=CARTESIAN_POINT('Ctrl Pts',(4.93943407798838,-3.77280013860123,6.47430161545231));
#18509=CARTESIAN_POINT('Ctrl Pts',(4.96712454271302,-4.27383503035714,6.54114965025572));
#18510=CARTESIAN_POINT('Ctrl Pts',(5.14782487662629,-4.62241497626213,6.59494409855566));
#18511=CARTESIAN_POINT('Ctrl Pts',(5.37295079462874,-4.86103853161568,6.63994694552246));
#18512=CARTESIAN_POINT('Ctrl Pts',(5.69611194962567,-5.03208597410825,6.68966723228357));
#18513=CARTESIAN_POINT('Ctrl Pts',(6.09404105102488,-5.07700452575227,6.74417783171338));
#18514=CARTESIAN_POINT('Ctrl Pts',(6.54806597605186,-4.95615077255924,6.80807397654506));
#18515=CARTESIAN_POINT('Ctrl Pts',(6.95984908440191,-4.58929774796911,6.88152070079881));
#18516=CARTESIAN_POINT('Ctrl Pts',(7.13324602081489,-3.98862814197939,6.96467721107475));
#18517=CARTESIAN_POINT('Ctrl Pts',(6.9598216073969,-3.38470802488132,7.04834227232992));
#18518=CARTESIAN_POINT('Ctrl Pts',(6.48881513689751,-2.96289006313062,7.13247292529825));
#18519=CARTESIAN_POINT('Ctrl Pts',(5.86248371502993,-2.85639547254553,7.21704160193825));
#18520=CARTESIAN_POINT('Ctrl Pts',(5.27257813080996,-3.10013645753721,7.30200242561844));
#18521=CARTESIAN_POINT('Ctrl Pts',(4.90156434344046,-3.62273164012634,7.38731106651996));
#18522=CARTESIAN_POINT('Ctrl Pts',(4.86488076919295,-4.26484215361151,7.47291989869636));
#18523=CARTESIAN_POINT('Ctrl Pts',(5.17689565992446,-4.82960611614006,7.55877747642911));
#18524=CARTESIAN_POINT('Ctrl Pts',(5.74278059709062,-5.14259803736158,7.64484502388108));
#18525=CARTESIAN_POINT('Ctrl Pts',(6.38962394316408,-5.1063947491349,7.73106975793031));
#18526=CARTESIAN_POINT('Ctrl Pts',(6.91886767714568,-4.73119514243953,7.81739789224607));
#18527=CARTESIAN_POINT('Ctrl Pts',(7.16697506945629,-4.13139347086528,7.90378793880489));
#18528=CARTESIAN_POINT('Ctrl Pts',(7.05840291902035,-3.49156698921832,7.99018524187825));
#18529=CARTESIAN_POINT('Ctrl Pts',(6.6259671749691,-3.00779841905544,8.07653128299141));
#18530=CARTESIAN_POINT('Ctrl Pts',(6.00342339258711,-2.82875695864265,8.16278221624947));
#18531=CARTESIAN_POINT('Ctrl Pts',(5.3816245849515,-3.00760289250318,8.24887562077341));
#18532=CARTESIAN_POINT('Ctrl Pts',(4.96793364487745,-3.47126919190322,8.33159562484918));
#18533=CARTESIAN_POINT('Ctrl Pts',(4.85154007935987,-4.05076879557578,8.41090797936888));
#18534=CARTESIAN_POINT('Ctrl Pts',(5.01800897195225,-4.59134836316443,8.48682542635688));
#18535=CARTESIAN_POINT('Ctrl Pts',(5.38828999036735,-4.95178056335741,8.55617651731747));
#18536=CARTESIAN_POINT('Ctrl Pts',(5.82439623786284,-5.10394949210358,8.61901205223471));
#18537=CARTESIAN_POINT('Ctrl Pts',(6.23842569304392,-5.08845315445427,8.6753812452482));
#18538=CARTESIAN_POINT('Ctrl Pts',(6.61685601287741,-4.92308289439992,8.73156765404928));
#18539=CARTESIAN_POINT('Ctrl Pts',(6.90771592127364,-4.63205020805392,8.78754987472152));
#18540=CARTESIAN_POINT('Ctrl Pts',(7.07151318879937,-4.2562632267042,8.84332122014839));
#18541=CARTESIAN_POINT('Ctrl Pts',(7.08662361123704,-3.84826122336414,8.89887039673394));
#18542=CARTESIAN_POINT('Ctrl Pts',(6.95218526115907,-3.46454996619298,8.95418779366907));
#18543=CARTESIAN_POINT('Ctrl Pts',(6.68800360958442,-3.15783352136326,9.00926396892089));
#18544=CARTESIAN_POINT('Ctrl Pts',(6.33164898032002,-2.96969809280073,9.06409031981465));
#18545=CARTESIAN_POINT('Ctrl Pts',(5.93307270473151,-2.92498136414862,9.11865878717923));
#18546=CARTESIAN_POINT('Ctrl Pts',(5.54760066898876,-3.028464827269,9.17296209959429));
#18547=CARTESIAN_POINT('Ctrl Pts',(5.22817429689392,-3.26445713236173,9.22699350570149));
#18548=CARTESIAN_POINT('Ctrl Pts',(5.01816505797095,-3.59907103783072,9.28074733097771));
#18549=CARTESIAN_POINT('Ctrl Pts',(4.94523109104339,-3.98531889354533,9.33421783283799));
#18550=CARTESIAN_POINT('Ctrl Pts',(5.01822063845842,-4.36924877748871,9.3874017867631));
#18551=CARTESIAN_POINT('Ctrl Pts',(5.24807831595622,-4.73508877868424,9.44617162792128));
#18552=CARTESIAN_POINT('Ctrl Pts',(5.65005396981199,-4.99449121289196,9.51039938577164));
#18553=CARTESIAN_POINT('Ctrl Pts',(6.16696735742553,-5.03242068584373,9.57993815379645));
#18554=CARTESIAN_POINT('Ctrl Pts',(6.52296885884133,-4.87140435012961,9.63241396136568));
#18555=CARTESIAN_POINT('Ctrl Pts',(6.71347179503556,-4.69592899910923,9.66817929864774));
#18556=CARTESIAN_POINT('Ctrl Pts',(6.83142515980489,-4.55217041674898,9.69387451281195));
#18557=CARTESIAN_POINT('Ctrl Pts',(6.98197740508559,-4.26180022510805,9.7386956488303));
#18558=CARTESIAN_POINT('Ctrl Pts',(7.00835664843526,-3.78482966702737,9.80230908785757));
#18559=CARTESIAN_POINT('Ctrl Pts',(6.73265925800214,-3.28750526053974,9.87798665633685));
#18560=CARTESIAN_POINT('Ctrl Pts',(6.23900967174894,-3.01545842822921,9.9530177739628));
#18561=CARTESIAN_POINT('Ctrl Pts',(5.68107426992735,-3.04754329136254,10.02741686381));
#18562=CARTESIAN_POINT('Ctrl Pts',(5.22919452226571,-3.36862150726833,10.1012057629823));
#18563=CARTESIAN_POINT('Ctrl Pts',(5.01940446719196,-3.87702307203514,10.1744097575186));
#18564=CARTESIAN_POINT('Ctrl Pts',(5.11135737798824,-4.41486364909888,10.2470495853014));
#18565=CARTESIAN_POINT('Ctrl Pts',(5.47273125967169,-4.81842416402667,10.3191579186434));
#18566=CARTESIAN_POINT('Ctrl Pts',(5.98976976867957,-4.96684498725752,10.3907666330935));
#18567=CARTESIAN_POINT('Ctrl Pts',(6.50319689175154,-4.81844594629322,10.4619122586038));
#18568=CARTESIAN_POINT('Ctrl Pts',(6.85686854910234,-4.4220387290267,10.5326333401887));
#18569=CARTESIAN_POINT('Ctrl Pts',(6.94499280492971,-3.90107632051501,10.6029711277556));
#18570=CARTESIAN_POINT('Ctrl Pts',(6.74345059478189,-3.41542481303838,10.6729692924891));
#18571=CARTESIAN_POINT('Ctrl Pts',(6.31626083963058,-3.11267459898931,10.742672972225));
#18572=CARTESIAN_POINT('Ctrl Pts',(5.79529421647195,-3.08367324798476,10.8121304684942));
#18573=CARTESIAN_POINT('Ctrl Pts',(5.34009144913045,-3.33549309978965,10.8813884178955));
#18574=CARTESIAN_POINT('Ctrl Pts',(5.08895191849142,-3.78995661189334,10.9505018220951));
#18575=CARTESIAN_POINT('Ctrl Pts',(5.11835951367094,-4.30749747225698,11.0195109289986));
#18576=CARTESIAN_POINT('Ctrl Pts',(5.41801944296879,-4.73002031986431,11.0884703947198));
#18577=CARTESIAN_POINT('Ctrl Pts',(5.89668467049593,-4.92825270792295,11.157438280058));
#18578=CARTESIAN_POINT('Ctrl Pts',(6.40782870093169,-4.84169521275955,11.2264591709475));
#18579=CARTESIAN_POINT('Ctrl Pts',(6.79515456050063,-4.4954187626051,11.2955952685095));
#18580=CARTESIAN_POINT('Ctrl Pts',(6.89129509472742,-4.16277368800117,11.3417786308327));
#18581=CARTESIAN_POINT('Ctrl Pts',(6.89131766144517,-3.99514256899045,11.3649203988529));
#18582=CARTESIAN_POINT('Ctrl Pts',(7.11181302032296,-4.0034772816564,2.72529728340312));
#18583=CARTESIAN_POINT('Ctrl Pts',(7.11178503697032,-3.795609668472,2.75399376949983));
#18584=CARTESIAN_POINT('Ctrl Pts',(6.99231662213726,-3.38176503061251,2.8114460028125));
#18585=CARTESIAN_POINT('Ctrl Pts',(6.51087276301266,-2.95155110950397,2.89735412612978));
#18586=CARTESIAN_POINT('Ctrl Pts',(5.87632413377557,-2.84418543881411,2.98303979398471));
#18587=CARTESIAN_POINT('Ctrl Pts',(5.2839166060325,-3.08988019972769,3.06841725271835));
#18588=CARTESIAN_POINT('Ctrl Pts',(4.91451380684877,-3.61116286149957,3.15345799266807));
#18589=CARTESIAN_POINT('Ctrl Pts',(4.87941312230243,-4.24603397475997,3.23810978758372));
#18590=CARTESIAN_POINT('Ctrl Pts',(5.18560875700521,-4.79977729807461,3.3223375500771));
#18591=CARTESIAN_POINT('Ctrl Pts',(5.73675144209106,-5.10364461823107,3.4061038382733));
#18592=CARTESIAN_POINT('Ctrl Pts',(6.36119748488511,-5.06806408189714,3.48936636705102));
#18593=CARTESIAN_POINT('Ctrl Pts',(6.86777018966466,-4.70793950062804,3.57209524538133));
#18594=CARTESIAN_POINT('Ctrl Pts',(7.10342410685789,-4.13743665807794,3.65425938248879));
#18595=CARTESIAN_POINT('Ctrl Pts',(7.00016590193463,-3.53336934983432,3.73583291487668));
#18596=CARTESIAN_POINT('Ctrl Pts',(6.59438611967027,-3.08027854269764,3.81679253233116));
#18597=CARTESIAN_POINT('Ctrl Pts',(6.01433584924907,-2.91387555126545,3.89711903146131));
#18598=CARTESIAN_POINT('Ctrl Pts',(5.43928254017653,-3.08021570651043,3.97679647255008));
#18599=CARTESIAN_POINT('Ctrl Pts',(5.05895974480875,-3.5069990781973,4.0528868562602));
#18600=CARTESIAN_POINT('Ctrl Pts',(4.96976763296824,-3.95237190959014,4.11385288434471));
#18601=CARTESIAN_POINT('Ctrl Pts',(5.0211552143318,-4.24201596307504,4.15426621773676));
#18602=CARTESIAN_POINT('Ctrl Pts',(5.08010879807319,-4.39785530700753,4.17729369334087));
#18603=CARTESIAN_POINT('Ctrl Pts',(5.19657114195399,-4.6184869703178,4.21176842639279));
#18604=CARTESIAN_POINT('Ctrl Pts',(5.47119125599088,-4.88607017711824,4.26322384295608));
#18605=CARTESIAN_POINT('Ctrl Pts',(5.95966222257167,-5.02298665218075,4.33131168944356));
#18606=CARTESIAN_POINT('Ctrl Pts',(6.45043526956446,-4.91056588865359,4.39887225762002));
#18607=CARTESIAN_POINT('Ctrl Pts',(6.79314941065994,-4.60696622071268,4.46032348296662));
#18608=CARTESIAN_POINT('Ctrl Pts',(6.9558334855932,-4.23292331056928,4.51582395385229));
#18609=CARTESIAN_POINT('Ctrl Pts',(6.96951025099049,-3.86809398252934,4.56548927299046));
#18610=CARTESIAN_POINT('Ctrl Pts',(6.84924354955551,-3.52565366333575,4.6148810745284));
#18611=CARTESIAN_POINT('Ctrl Pts',(6.58767150103308,-3.22134137372009,4.66946015528846));
#18612=CARTESIAN_POINT('Ctrl Pts',(6.18235541401055,-3.0388990108291,4.72912598691042));
#18613=CARTESIAN_POINT('Ctrl Pts',(5.70197393505759,-3.07534404320876,4.79377090669685));
#18614=CARTESIAN_POINT('Ctrl Pts',(5.38416977230659,-3.28116084516777,4.8445902293805));
#18615=CARTESIAN_POINT('Ctrl Pts',(5.21966595419117,-3.49597856977572,4.88188785520888));
#18616=CARTESIAN_POINT('Ctrl Pts',(5.11528011960377,-3.70245947496454,4.91378229331294));
#18617=CARTESIAN_POINT('Ctrl Pts',(5.06106882547897,-3.98943465448296,4.95351375393308));
#18618=CARTESIAN_POINT('Ctrl Pts',(5.12618530561125,-4.33220315307956,5.00098440504624));
#18619=CARTESIAN_POINT('Ctrl Pts',(5.31109273276004,-4.62645525277273,5.04825832289593));
#18620=CARTESIAN_POINT('Ctrl Pts',(5.5896728391335,-4.8317388157924,5.09534903382872));
#18621=CARTESIAN_POINT('Ctrl Pts',(5.92295480412722,-4.92113185558065,5.14227041620987));
#18622=CARTESIAN_POINT('Ctrl Pts',(6.26421131547055,-4.88225344620643,5.18903417313737));
#18623=CARTESIAN_POINT('Ctrl Pts',(6.66909695604073,-4.66950391227245,5.25119574478853));
#18624=CARTESIAN_POINT('Ctrl Pts',(6.96872410809086,-4.15143760418596,5.32855257233037));
#18625=CARTESIAN_POINT('Ctrl Pts',(6.8085865206455,-3.45225571131928,5.42097838800836));
#18626=CARTESIAN_POINT('Ctrl Pts',(6.31714251855204,-3.1186633455213,5.49774585582468));
#18627=CARTESIAN_POINT('Ctrl Pts',(5.86618303936299,-3.10330610067415,5.55908145139043));
#18628=CARTESIAN_POINT('Ctrl Pts',(5.51181006773901,-3.22658005086454,5.61016213242431));
#18629=CARTESIAN_POINT('Ctrl Pts',(5.21202969008444,-3.5188532387546,5.66633081666598));
#18630=CARTESIAN_POINT('Ctrl Pts',(5.07759303828484,-3.95538499461575,5.72761250189965));
#18631=CARTESIAN_POINT('Ctrl Pts',(5.15296720022287,-4.32855327746985,5.77872934943021));
#18632=CARTESIAN_POINT('Ctrl Pts',(5.29475280348604,-4.54747613431151,5.81454405119438));
#18633=CARTESIAN_POINT('Ctrl Pts',(5.39688304163522,-4.65482873693581,5.83502588408689));
#18634=CARTESIAN_POINT('Ctrl Pts',(5.56892779389234,-4.79583961287311,5.86576115556887));
#18635=CARTESIAN_POINT('Ctrl Pts',(5.88894832539248,-4.9215688629896,5.91191769336285));
#18636=CARTESIAN_POINT('Ctrl Pts',(6.30708827323726,-4.86933300302203,5.96847220906027));
#18637=CARTESIAN_POINT('Ctrl Pts',(6.62788735520902,-4.66753190240589,6.02001845773736));
#18638=CARTESIAN_POINT('Ctrl Pts',(6.83101003502994,-4.39254735889121,6.06654237092183));
#18639=CARTESIAN_POINT('Ctrl Pts',(6.91988771324996,-4.06130312576411,6.11319476549568));
#18640=CARTESIAN_POINT('Ctrl Pts',(6.88148404501785,-3.71943526644181,6.15999913034724));
#18641=CARTESIAN_POINT('Ctrl Pts',(6.72018765865318,-3.41426217881823,6.2069633667072));
#18642=CARTESIAN_POINT('Ctrl Pts',(6.45771684783584,-3.18804833433947,6.25410242444302));
#18643=CARTESIAN_POINT('Ctrl Pts',(6.12942429058675,-3.07326355575574,6.30142649923685));
#18644=CARTESIAN_POINT('Ctrl Pts',(5.72212261020255,-3.0879652583245,6.35687278657594));
#18645=CARTESIAN_POINT('Ctrl Pts',(5.30280188330194,-3.31834662771335,6.4205824119603));
#18646=CARTESIAN_POINT('Ctrl Pts',(5.04015910673608,-3.79329231273531,6.49276455500539));
#18647=CARTESIAN_POINT('Ctrl Pts',(5.06529254998145,-4.24752611947387,6.55336865808706));
#18648=CARTESIAN_POINT('Ctrl Pts',(5.229105522544,-4.56352145996701,6.60213508583633));
#18649=CARTESIAN_POINT('Ctrl Pts',(5.43321055638464,-4.7798606832403,6.64293592276993));
#18650=CARTESIAN_POINT('Ctrl Pts',(5.72627515597292,-4.93498617020499,6.68802792013858));
#18651=CARTESIAN_POINT('Ctrl Pts',(6.08735128746861,-4.97576489038208,6.73749113160384));
#18652=CARTESIAN_POINT('Ctrl Pts',(6.49967356053982,-4.86604225236812,6.7955213010878));
#18653=CARTESIAN_POINT('Ctrl Pts',(6.87420709747073,-4.53253993649614,6.86231193633499));
#18654=CARTESIAN_POINT('Ctrl Pts',(7.03239424791724,-3.98519320250181,6.9381046731321));
#18655=CARTESIAN_POINT('Ctrl Pts',(6.8741451200112,-3.43332696122199,7.01455824015083));
#18656=CARTESIAN_POINT('Ctrl Pts',(6.44261208450338,-3.04651151223732,7.09168325300931));
#18657=CARTESIAN_POINT('Ctrl Pts',(5.86655717868025,-2.94824980040446,7.16947724567467));
#18658=CARTESIAN_POINT('Ctrl Pts',(5.32167885280403,-3.17302008183712,7.24794249190133));
#18659=CARTESIAN_POINT('Ctrl Pts',(4.97724918654381,-3.65751078947094,7.3270742884974));
#18660=CARTESIAN_POINT('Ctrl Pts',(4.94266353869487,-4.25587662754318,7.40686673243344));
#18661=CARTESIAN_POINT('Ctrl Pts',(5.23454234061227,-4.78511199353983,7.48731081374599));
#18662=CARTESIAN_POINT('Ctrl Pts',(5.76723695574062,-5.08027341466217,7.56838248480538));
#18663=CARTESIAN_POINT('Ctrl Pts',(6.37988233163738,-5.04648348782411,7.65006374692676));
#18664=CARTESIAN_POINT('Ctrl Pts',(6.88440160593799,-4.68944269844362,7.73233497259739));
#18665=CARTESIAN_POINT('Ctrl Pts',(7.12272965880694,-4.11471198609239,7.81515815314353));
#18666=CARTESIAN_POINT('Ctrl Pts',(7.01854737810762,-3.49745445431086,7.89850602421412));
#18667=CARTESIAN_POINT('Ctrl Pts',(6.59913665512866,-3.02739537215762,7.98235325668356));
#18668=CARTESIAN_POINT('Ctrl Pts',(5.99089552939524,-2.85185547830102,8.0666537355345));
#18669=CARTESIAN_POINT('Ctrl Pts',(5.37895087333546,-3.02724577484401,8.15138435106854));
#18670=CARTESIAN_POINT('Ctrl Pts',(4.96873838061378,-3.4861291063974,8.23332981304256));
#18671=CARTESIAN_POINT('Ctrl Pts',(4.85223629310714,-4.06382045547982,8.31242873092161));
#18672=CARTESIAN_POINT('Ctrl Pts',(5.01879225277718,-4.60612524072465,8.38858506420336));
#18673=CARTESIAN_POINT('Ctrl Pts',(5.39215287487895,-4.9701201364919,8.45857688050792));
#18674=CARTESIAN_POINT('Ctrl Pts',(5.83447254628042,-5.12466841834738,8.52232192406592));
#18675=CARTESIAN_POINT('Ctrl Pts',(6.25638035377061,-5.1090579638618,8.57978038495634));
#18676=CARTESIAN_POINT('Ctrl Pts',(6.64376737701431,-4.93997081523902,8.63729012374795));
#18677=CARTESIAN_POINT('Ctrl Pts',(6.94290952660399,-4.6409000426499,8.69485452773811));
#18678=CARTESIAN_POINT('Ctrl Pts',(7.11219528325435,-4.25296279440545,8.75244998619474));
#18679=CARTESIAN_POINT('Ctrl Pts',(7.12803866414581,-3.82988735801254,8.8100627820474));
#18680=CARTESIAN_POINT('Ctrl Pts',(6.98820455924593,-3.43025618594452,8.86767703449591));
#18681=CARTESIAN_POINT('Ctrl Pts',(6.71208792131979,-3.10942500354523,8.92527773350626));
#18682=CARTESIAN_POINT('Ctrl Pts',(6.33802625218942,-2.91175521399945,8.98284944887227));
#18683=CARTESIAN_POINT('Ctrl Pts',(5.91791836782838,-2.86446190085055,9.04037715807962));
#18684=CARTESIAN_POINT('Ctrl Pts',(5.50999816880691,-2.97381056092891,9.09784552911978));
#18685=CARTESIAN_POINT('Ctrl Pts',(5.1706475163805,-3.22433555582723,9.1552402121433));
#18686=CARTESIAN_POINT('Ctrl Pts',(4.94666850851543,-3.58093351744638,9.21254527965908));
#18687=CARTESIAN_POINT('Ctrl Pts',(4.86851194638551,-3.9940613147631,9.2697490146684));
#18688=CARTESIAN_POINT('Ctrl Pts',(4.94671706804593,-4.40612531487305,9.32683105079786));
#18689=CARTESIAN_POINT('Ctrl Pts',(5.19406373867607,-4.80007560428671,9.39010930326567));
#18690=CARTESIAN_POINT('Ctrl Pts',(5.62823706810774,-5.08055728128927,9.45950840910193));
#18691=CARTESIAN_POINT('Ctrl Pts',(6.18883171995305,-5.12196510699354,9.53493153509677));
#18692=CARTESIAN_POINT('Ctrl Pts',(6.57630879888758,-4.94690033774589,9.59203839047609));
#18693=CARTESIAN_POINT('Ctrl Pts',(6.78403797218043,-4.75557641911101,9.63103661249943));
#18694=CARTESIAN_POINT('Ctrl Pts',(6.91276029943424,-4.59870147295395,9.65907726902172));
#18695=CARTESIAN_POINT('Ctrl Pts',(7.07729956347344,-4.28147376753379,9.70805109539169));
#18696=CARTESIAN_POINT('Ctrl Pts',(7.10639635228469,-3.75916764163223,9.77771384283918));
#18697=CARTESIAN_POINT('Ctrl Pts',(6.80391089471105,-3.21307570521622,9.86079704272353));
#18698=CARTESIAN_POINT('Ctrl Pts',(6.2609409806921,-2.91366124263847,9.94333528846695));
#18699=CARTESIAN_POINT('Ctrl Pts',(5.64625305798367,-2.94889736194364,10.0253000041248));
#18700=CARTESIAN_POINT('Ctrl Pts',(5.14790701284458,-3.30290571674617,10.1066660051286));
#18701=CARTESIAN_POINT('Ctrl Pts',(4.91646375369252,-3.86373001111236,10.1874119824758));
#18702=CARTESIAN_POINT('Ctrl Pts',(5.01790999463095,-4.45690610328577,10.2675187444275));
#18703=CARTESIAN_POINT('Ctrl Pts',(5.4162045723001,-4.90156974945713,10.3469724146488));
#18704=CARTESIAN_POINT('Ctrl Pts',(5.98520329484128,-5.0647656683169,10.4257622661485));
#18705=CARTESIAN_POINT('Ctrl Pts',(6.54898949352491,-4.90161790412091,10.5038818275361));
#18706=CARTESIAN_POINT('Ctrl Pts',(6.93618330712169,-4.4672853226491,10.5813283621489));
#18707=CARTESIAN_POINT('Ctrl Pts',(7.0321116791204,-3.89849452357714,10.6581033369473));
#18708=CARTESIAN_POINT('Ctrl Pts',(6.81262813853771,-3.37046494817674,10.7342117384801));
#18709=CARTESIAN_POINT('Ctrl Pts',(6.34989485304325,-3.04297798221524,10.8096633648087));
#18710=CARTESIAN_POINT('Ctrl Pts',(5.78863332577001,-3.01213943792801,10.8844698528756));
#18711=CARTESIAN_POINT('Ctrl Pts',(5.30116720621585,-3.28231261460185,10.958651011249));
#18712=CARTESIAN_POINT('Ctrl Pts',(5.03414065496795,-3.76648217455745,11.0322203362354));
#18713=CARTESIAN_POINT('Ctrl Pts',(5.0657612686785,-4.31399257613907,11.1052167694189));
#18714=CARTESIAN_POINT('Ctrl Pts',(5.38103274839073,-4.75764250667029,11.1776583648672));
#18715=CARTESIAN_POINT('Ctrl Pts',(5.88048241165544,-4.96386839430271,11.2495801905597));
#18716=CARTESIAN_POINT('Ctrl Pts',(6.40941698618055,-4.87375847765753,11.3209983713259));
#18717=CARTESIAN_POINT('Ctrl Pts',(6.80673213210873,-4.51761905992164,11.3919962517265));
#18718=CARTESIAN_POINT('Ctrl Pts',(6.90419755947852,-4.17887731899267,11.4389950778511));
#18719=CARTESIAN_POINT('Ctrl Pts',(6.90422048036531,-4.00861534543431,11.4625000399251));
#18720=CARTESIAN_POINT('Ctrl Pts',(7.08935434998871,-3.99023209767526,2.62933176205122));
#18721=CARTESIAN_POINT('Ctrl Pts',(7.08932688285949,-3.78619912616226,2.65749886918541));
#18722=CARTESIAN_POINT('Ctrl Pts',(6.97225742007367,-3.37929495075464,2.71396227449415));
#18723=CARTESIAN_POINT('Ctrl Pts',(6.4959395448978,-2.95271134548437,2.79904118774148));
#18724=CARTESIAN_POINT('Ctrl Pts',(5.86342126244207,-2.84513906790044,2.88445011210575));
#18725=CARTESIAN_POINT('Ctrl Pts',(5.26853596979891,-3.09120074560871,2.97014778749716));
#18726=CARTESIAN_POINT('Ctrl Pts',(4.89471164796743,-3.61770953674116,3.05608476471754));
#18727=CARTESIAN_POINT('Ctrl Pts',(4.85840821685399,-4.26367377675506,3.1422138288304));
#18728=CARTESIAN_POINT('Ctrl Pts',(5.17152956425176,-4.83116889517306,3.22848321087116));
#18729=CARTESIAN_POINT('Ctrl Pts',(5.73952231760977,-5.1449839685189,3.3148407995635));
#18730=CARTESIAN_POINT('Ctrl Pts',(6.38756274099376,-5.10862866433251,3.40123877203696));
#18731=CARTESIAN_POINT('Ctrl Pts',(6.91687976395631,-4.73301508245801,3.48762382685246));
#18732=CARTESIAN_POINT('Ctrl Pts',(7.16496045282747,-4.13383039277197,3.57394514348085));
#18733=CARTESIAN_POINT('Ctrl Pts',(7.05634188199328,-3.49536193020094,3.66015119897581));
#18734=CARTESIAN_POINT('Ctrl Pts',(6.62546157536257,-3.01351480304848,3.74619172902684));
#18735=CARTESIAN_POINT('Ctrl Pts',(6.00584453576659,-2.83528701623401,3.83201712057257));
#18736=CARTESIAN_POINT('Ctrl Pts',(5.38823156605757,-3.01349570186831,3.91757943615934));
#18737=CARTESIAN_POINT('Ctrl Pts',(4.9776391918564,-3.47368186406432,3.99967416531157));
#18738=CARTESIAN_POINT('Ctrl Pts',(4.88081244001865,-3.95609746742031,4.06572132496842));
#18739=CARTESIAN_POINT('Ctrl Pts',(4.93659467832656,-4.27068186833768,4.1096153344438));
#18740=CARTESIAN_POINT('Ctrl Pts',(5.00069912947771,-4.44014510684179,4.13465648931247));
#18741=CARTESIAN_POINT('Ctrl Pts',(5.12743957449684,-4.6802586444565,4.17217678554748));
#18742=CARTESIAN_POINT('Ctrl Pts',(5.42683993188746,-4.97217063644552,4.22830517648922));
#18743=CARTESIAN_POINT('Ctrl Pts',(5.96096699897456,-5.12206279818076,4.30276781882196));
#18744=CARTESIAN_POINT('Ctrl Pts',(6.49902876152345,-4.99896356644126,4.37684117025936));
#18745=CARTESIAN_POINT('Ctrl Pts',(6.87559825091274,-4.66549634791073,4.44436497611438));
#18746=CARTESIAN_POINT('Ctrl Pts',(7.05461408495889,-4.25402036572474,4.50542661030662));
#18747=CARTESIAN_POINT('Ctrl Pts',(7.06969558189068,-3.85224672374576,4.56013139070142));
#18748=CARTESIAN_POINT('Ctrl Pts',(6.93717502307927,-3.47483694654967,4.61457295672824));
#18749=CARTESIAN_POINT('Ctrl Pts',(6.64875041917917,-3.13927424785343,4.67476637000182));
#18750=CARTESIAN_POINT('Ctrl Pts',(6.20170223313162,-2.93804341964427,4.74058490002232));
#18751=CARTESIAN_POINT('Ctrl Pts',(5.67192221372407,-2.978262942237,4.81188320877822));
#18752=CARTESIAN_POINT('Ctrl Pts',(5.3215938512512,-3.2052069184109,4.86793754222562));
#18753=CARTESIAN_POINT('Ctrl Pts',(5.14042083624559,-3.44180714820557,4.90902121836561));
#18754=CARTESIAN_POINT('Ctrl Pts',(5.02550641655777,-3.66912250596354,4.94413847804827));
#18755=CARTESIAN_POINT('Ctrl Pts',(4.9659167911861,-3.98480613469966,4.98785114911865));
#18756=CARTESIAN_POINT('Ctrl Pts',(5.03749702385629,-4.36134884281863,5.04000993703854));
#18757=CARTESIAN_POINT('Ctrl Pts',(5.24037015462402,-4.68404809620616,5.09187198427612));
#18758=CARTESIAN_POINT('Ctrl Pts',(5.54537654264952,-4.90873413606796,5.14343592097922));
#18759=CARTESIAN_POINT('Ctrl Pts',(5.909472076432,-5.00629854924447,5.194701131758));
#18760=CARTESIAN_POINT('Ctrl Pts',(6.28132398727991,-4.96385799414479,5.24566981818468));
#18761=CARTESIAN_POINT('Ctrl Pts',(6.72130577810205,-4.73250966468848,5.31323388597859));
#18762=CARTESIAN_POINT('Ctrl Pts',(7.04489872138567,-4.17152523185947,5.39697306163749));
#18763=CARTESIAN_POINT('Ctrl Pts',(6.87173413710806,-3.42039959502914,5.49631993121801));
#18764=CARTESIAN_POINT('Ctrl Pts',(6.34720530709739,-3.06549796425185,5.57820768068278));
#18765=CARTESIAN_POINT('Ctrl Pts',(5.86953086171109,-3.04944298539597,5.64319531743515));
#18766=CARTESIAN_POINT('Ctrl Pts',(5.49584975715717,-3.17960634615903,5.69707450016525));
#18767=CARTESIAN_POINT('Ctrl Pts',(5.18167374083759,-3.48641160818447,5.75599838207982));
#18768=CARTESIAN_POINT('Ctrl Pts',(5.04197029026427,-3.94140910039868,5.81987647010874));
#18769=CARTESIAN_POINT('Ctrl Pts',(5.12029863594809,-4.32753826506529,5.87278413743482));
#18770=CARTESIAN_POINT('Ctrl Pts',(5.2663149982563,-4.55288629523623,5.90966649482064));
#18771=CARTESIAN_POINT('Ctrl Pts',(5.37117741816517,-4.66310330254181,5.93069699853573));
#18772=CARTESIAN_POINT('Ctrl Pts',(5.54752519184094,-4.80762211066538,5.96220176022617));
#18773=CARTESIAN_POINT('Ctrl Pts',(5.87417596723426,-4.93562642650329,6.00930677655604));
#18774=CARTESIAN_POINT('Ctrl Pts',(6.29769637485263,-4.88232598337754,6.06660612467952));
#18775=CARTESIAN_POINT('Ctrl Pts',(6.62047379630039,-4.67906087756066,6.11850395269178));
#18776=CARTESIAN_POINT('Ctrl Pts',(6.82362142151304,-4.4037527855136,6.16506694041442));
#18777=CARTESIAN_POINT('Ctrl Pts',(6.91192017974991,-4.07401150590665,6.21150986460091));
#18778=CARTESIAN_POINT('Ctrl Pts',(6.87373604354229,-3.73565491190597,6.25784046646843));
#18779=CARTESIAN_POINT('Ctrl Pts',(6.71481960446947,-3.43533167367221,6.3040764125896));
#18780=CARTESIAN_POINT('Ctrl Pts',(6.45774003972392,-3.21399047925324,6.35023076864715));
#18781=CARTESIAN_POINT('Ctrl Pts',(6.13801384513281,-3.10236364071456,6.39631970034203));
#18782=CARTESIAN_POINT('Ctrl Pts',(5.74348593015072,-3.11679890656582,6.45002812788936));
#18783=CARTESIAN_POINT('Ctrl Pts',(5.34012414260463,-3.33894846419464,6.51135232543338));
#18784=CARTESIAN_POINT('Ctrl Pts',(5.08970971672879,-3.79287801839994,6.5803109175142));
#18785=CARTESIAN_POINT('Ctrl Pts',(5.11394525582943,-4.22367302794002,6.63779297160539));
#18786=CARTESIAN_POINT('Ctrl Pts',(5.26859250522411,-4.52182198991263,6.68381562742008));
#18787=CARTESIAN_POINT('Ctrl Pts',(5.46062438052977,-4.72528715932241,6.7221950091176));
#18788=CARTESIAN_POINT('Ctrl Pts',(5.73533948531848,-4.87056941349058,6.76445662901709));
#18789=CARTESIAN_POINT('Ctrl Pts',(6.07241401329558,-4.90852365400217,6.81063041932966));
#18790=CARTESIAN_POINT('Ctrl Pts',(6.45585514108403,-4.80634676067811,6.8645984283862));
#18791=CARTESIAN_POINT('Ctrl Pts',(6.80245047206153,-4.49730107889992,6.92644266376476));
#18792=CARTESIAN_POINT('Ctrl Pts',(6.94792656407525,-3.99279744060583,6.99628588167397));
#18793=CARTESIAN_POINT('Ctrl Pts',(6.80243409723874,-3.48638510759692,7.06644845435211));
#18794=CARTESIAN_POINT('Ctrl Pts',(6.40764162124333,-3.13281085464808,7.13697136148438));
#18795=CARTESIAN_POINT('Ctrl Pts',(5.88234601693467,-3.04340282592901,7.20790251461747));
#18796=CARTESIAN_POINT('Ctrl Pts',(5.38671136540327,-3.24801639362842,7.27927901227808));
#18797=CARTESIAN_POINT('Ctrl Pts',(5.0740013431706,-3.68807082076264,7.35113797216885));
#18798=CARTESIAN_POINT('Ctrl Pts',(5.04267804088376,-4.2308763596221,7.42351167554797));
#18799=CARTESIAN_POINT('Ctrl Pts',(5.30731187114947,-4.71069600094691,7.49642855210674));
#18800=CARTESIAN_POINT('Ctrl Pts',(5.79029962646666,-4.97836689832941,7.56992328530873));
#18801=CARTESIAN_POINT('Ctrl Pts',(6.34616999591135,-4.94778675880538,7.6440187765564));
#18802=CARTESIAN_POINT('Ctrl Pts',(6.80455108078886,-4.62356423479621,7.71873312942426));
#18803=CARTESIAN_POINT('Ctrl Pts',(7.02159429958252,-4.10059489849228,7.79409235639335));
#18804=CARTESIAN_POINT('Ctrl Pts',(6.92677315546898,-3.53754527937747,7.87010761270296));
#18805=CARTESIAN_POINT('Ctrl Pts',(6.54335772488925,-3.10743806009348,7.94678244740374));
#18806=CARTESIAN_POINT('Ctrl Pts',(5.98529704655144,-2.94609162323264,8.02413006489736));
#18807=CARTESIAN_POINT('Ctrl Pts',(5.42164916618205,-3.10728509594054,8.10214039646089));
#18808=CARTESIAN_POINT('Ctrl Pts',(5.04202949373677,-3.53143448190436,8.17791337266471));
#18809=CARTESIAN_POINT('Ctrl Pts',(4.93356821182761,-4.06783639076264,8.2513417969401));
#18810=CARTESIAN_POINT('Ctrl Pts',(5.08862282161157,-4.57369791196422,8.32235735676531));
#18811=CARTESIAN_POINT('Ctrl Pts',(5.43823576048116,-4.91492383754914,8.38792025541212));
#18812=CARTESIAN_POINT('Ctrl Pts',(5.85433946781558,-5.06047867538894,8.44788715643451));
#18813=CARTESIAN_POINT('Ctrl Pts',(6.25271887238557,-5.04587511822749,8.50212325209872));
#18814=CARTESIAN_POINT('Ctrl Pts',(6.61999951562128,-4.88572034405795,8.55663424769427));
#18815=CARTESIAN_POINT('Ctrl Pts',(6.90476939932178,-4.60122727426364,8.61139993288472));
#18816=CARTESIAN_POINT('Ctrl Pts',(7.06665260714968,-4.23063194099307,8.66641839038366));
#18817=CARTESIAN_POINT('Ctrl Pts',(7.08200568370839,-3.82474181939741,8.72168000590468));
#18818=CARTESIAN_POINT('Ctrl Pts',(6.947433257179,-3.43967321822155,8.7771760282935));
#18819=CARTESIAN_POINT('Ctrl Pts',(6.68039689961518,-3.12914741165085,8.83289647602786));
#18820=CARTESIAN_POINT('Ctrl Pts',(6.31697702825656,-2.93691623733113,8.88883108316005));
#18821=CARTESIAN_POINT('Ctrl Pts',(5.90695860513133,-2.89059061296164,8.94496880460782));
#18822=CARTESIAN_POINT('Ctrl Pts',(5.50700490680685,-2.99762875074735,9.0012983390224));
#18823=CARTESIAN_POINT('Ctrl Pts',(5.17272540838232,-3.24419480617616,9.05780734478288));
#18824=CARTESIAN_POINT('Ctrl Pts',(4.95102157956017,-3.59685017820169,9.11448414857256));
#18825=CARTESIAN_POINT('Ctrl Pts',(4.87318814711464,-4.00732421615173,9.17131408794555));
#18826=CARTESIAN_POINT('Ctrl Pts',(4.95108701817399,-4.41868857022641,9.22828780042604));
#18827=CARTESIAN_POINT('Ctrl Pts',(5.19894039635913,-4.81381967302136,9.29173363197765));
#18828=CARTESIAN_POINT('Ctrl Pts',(5.63639590476303,-5.09688098930182,9.36168596521111));
#18829=CARTESIAN_POINT('Ctrl Pts',(6.20488341287629,-5.13929550996791,9.43816289043042));
#18830=CARTESIAN_POINT('Ctrl Pts',(6.60031943017411,-4.96097203670386,9.49642064148387));
#18831=CARTESIAN_POINT('Ctrl Pts',(6.8130702619607,-4.76504447047869,9.5363558838958));
#18832=CARTESIAN_POINT('Ctrl Pts',(6.94511802689851,-4.60412809383265,9.56511887960774));
#18833=CARTESIAN_POINT('Ctrl Pts',(7.11437864669289,-4.27798597899338,9.61547396389942));
#18834=CARTESIAN_POINT('Ctrl Pts',(7.14491779222484,-3.73829148440297,9.68745604502794));
#18835=CARTESIAN_POINT('Ctrl Pts',(6.83083864734627,-3.17009688337909,9.77385551909786));
#18836=CARTESIAN_POINT('Ctrl Pts',(6.26290699701676,-2.8562934070938,9.86022492860254));
#18837=CARTESIAN_POINT('Ctrl Pts',(5.61575197634126,-2.89286502547761,9.94651247809435));
#18838=CARTESIAN_POINT('Ctrl Pts',(5.08778619204425,-3.26729393662258,10.0326676206064));
#18839=CARTESIAN_POINT('Ctrl Pts',(4.84092188303821,-3.86424218979877,10.1186403336879));
#18840=CARTESIAN_POINT('Ctrl Pts',(4.94906070406917,-4.49919530585996,10.2043810035239));
#18841=CARTESIAN_POINT('Ctrl Pts',(5.37714255217191,-4.97773968110716,10.2898422024077));
#18842=CARTESIAN_POINT('Ctrl Pts',(5.99182700819212,-5.15443673839473,10.3749777902456));
#18843=CARTESIAN_POINT('Ctrl Pts',(6.6036286643445,-4.9777550601931,10.4597437013092));
#18844=CARTESIAN_POINT('Ctrl Pts',(7.02554665450114,-4.50493359335247,10.5440980117182));
#18845=CARTESIAN_POINT('Ctrl Pts',(7.13063227624352,-3.88344998774725,10.6280012139768));
#18846=CARTESIAN_POINT('Ctrl Pts',(6.890317183568,-3.30472348185151,10.7114166464371));
#18847=CARTESIAN_POINT('Ctrl Pts',(6.38212732946614,-2.9448499039503,10.7943101163743));
#18848=CARTESIAN_POINT('Ctrl Pts',(5.76446732461662,-2.9107896777846,10.8766515375219));
#18849=CARTESIAN_POINT('Ctrl Pts',(5.22726169429406,-3.20844365100958,10.958411932489));
#18850=CARTESIAN_POINT('Ctrl Pts',(4.93276927196662,-3.74240011088686,11.0395707404944));
#18851=CARTESIAN_POINT('Ctrl Pts',(4.96767361997263,-4.34631263085527,11.1201000860987));
#18852=CARTESIAN_POINT('Ctrl Pts',(5.31535533916341,-4.83541600550362,11.1999832745146));
#18853=CARTESIAN_POINT('Ctrl Pts',(5.86556113061819,-5.06246353418302,11.2792176122038));
#18854=CARTESIAN_POINT('Ctrl Pts',(6.44726148398534,-4.96317297736691,11.3577766442642));
#18855=CARTESIAN_POINT('Ctrl Pts',(6.88312582385536,-4.57225455833006,11.4356903944807));
#18856=CARTESIAN_POINT('Ctrl Pts',(6.98969410226672,-4.20147268401305,11.4871431260612));
#18857=CARTESIAN_POINT('Ctrl Pts',(6.98971912848012,-4.01557182757373,11.5128070631624));
#18858=CARTESIAN_POINT('Ctrl Pts',(7.02991808875672,-3.9863204986747,2.60093950625054));
#18859=CARTESIAN_POINT('Ctrl Pts',(7.0298920767563,-3.79309660190507,2.62761440178745));
#18860=CARTESIAN_POINT('Ctrl Pts',(6.91909382179967,-3.40769064837915,2.68109050706102));
#18861=CARTESIAN_POINT('Ctrl Pts',(6.46676608976936,-3.00219879487548,2.76192331287528));
#18862=CARTESIAN_POINT('Ctrl Pts',(5.86416835249228,-2.89947315565633,2.84329274697736));
#18863=CARTESIAN_POINT('Ctrl Pts',(5.29547823170544,-3.13436399239426,2.92520207327125));
#18864=CARTESIAN_POINT('Ctrl Pts',(4.93671383355777,-3.63910836719776,3.00761460452821));
#18865=CARTESIAN_POINT('Ctrl Pts',(4.90144022313547,-4.26079346404597,3.09050869847464));
#18866=CARTESIAN_POINT('Ctrl Pts',(5.20362252301616,-4.80919944690218,3.17384785225833));
#18867=CARTESIAN_POINT('Ctrl Pts',(5.75431021582355,-5.11388475786273,3.25759644032169));
#18868=CARTESIAN_POINT('Ctrl Pts',(6.38540320153558,-5.07886240663714,3.34172581662129));
#18869=CARTESIAN_POINT('Ctrl Pts',(6.90325242066822,-4.71186766302553,3.42619408052645));
#18870=CARTESIAN_POINT('Ctrl Pts',(7.14727039378041,-4.12354721671033,3.51096234986392));
#18871=CARTESIAN_POINT('Ctrl Pts',(7.04052980174623,-3.49366540997803,3.59598782843037));
#18872=CARTESIAN_POINT('Ctrl Pts',(6.61390657684921,-3.01594762654595,3.6812269984434));
#18873=CARTESIAN_POINT('Ctrl Pts',(5.9973096813911,-2.83814561164906,3.76663507596031));
#18874=CARTESIAN_POINT('Ctrl Pts',(5.37968234307175,-3.01590762291788,3.85216530550586));
#18875=CARTESIAN_POINT('Ctrl Pts',(4.96698506179213,-3.47783712150818,3.9346017628615));
#18876=CARTESIAN_POINT('Ctrl Pts',(4.86906342867886,-3.96439384809991,4.0012048778156));
#18877=CARTESIAN_POINT('Ctrl Pts',(4.92546013389047,-4.28269662274511,4.04560996804786));
#18878=CARTESIAN_POINT('Ctrl Pts',(4.990412763925,-4.45442047509628,4.07098315160127));
#18879=CARTESIAN_POINT('Ctrl Pts',(5.11895625152796,-4.6979784138749,4.10903845085798));
#18880=CARTESIAN_POINT('Ctrl Pts',(5.42317137440073,-4.99492329369231,4.16607662934805));
#18881=CARTESIAN_POINT('Ctrl Pts',(5.968352558652,-5.14822243535607,4.2420839301269));
#18882=CARTESIAN_POINT('Ctrl Pts',(6.51978304095379,-5.02234952447351,4.31797503338202));
#18883=CARTESIAN_POINT('Ctrl Pts',(6.9072832001042,-4.67955144327851,4.38740393573842));
#18884=CARTESIAN_POINT('Ctrl Pts',(7.09212835650512,-4.25495690058516,4.45041049887341));
#18885=CARTESIAN_POINT('Ctrl Pts',(7.10785181269314,-3.83924601052615,4.50699939833727));
#18886=CARTESIAN_POINT('Ctrl Pts',(6.97044503028521,-3.44765854135089,4.56346997832381));
#18887=CARTESIAN_POINT('Ctrl Pts',(6.67054717410501,-3.09855890921501,4.62606392322435));
#18888=CARTESIAN_POINT('Ctrl Pts',(6.20426157743975,-2.88844544026138,4.69471395250901));
#18889=CARTESIAN_POINT('Ctrl Pts',(5.64980765832729,-2.9303193519752,4.76932248356804));
#18890=CARTESIAN_POINT('Ctrl Pts',(5.2820875278432,-3.16834842314897,4.82810745942499));
#18891=CARTESIAN_POINT('Ctrl Pts',(5.09152989701439,-3.41718119774718,4.87131005699247));
#18892=CARTESIAN_POINT('Ctrl Pts',(4.97054323829609,-3.65648857388211,4.9082745060722));
#18893=CARTESIAN_POINT('Ctrl Pts',(4.90764740745214,-3.98932272899894,4.95435456202079));
#18894=CARTESIAN_POINT('Ctrl Pts',(4.98320524804316,-4.38709184426172,5.00944034588392));
#18895=CARTESIAN_POINT('Ctrl Pts',(5.19781986825172,-4.72860825805215,5.06430729650093));
#18896=CARTESIAN_POINT('Ctrl Pts',(5.52108471179064,-4.96679238484029,5.11894800494866));
#18897=CARTESIAN_POINT('Ctrl Pts',(5.90757483068251,-5.07041839122686,5.17335835282008));
#18898=CARTESIAN_POINT('Ctrl Pts',(6.30287112434244,-5.02533471611233,5.22752888227952));
#18899=CARTESIAN_POINT('Ctrl Pts',(6.77118875319483,-4.77916066880441,5.29943161761435));
#18900=CARTESIAN_POINT('Ctrl Pts',(7.11631632438462,-4.18127802959054,5.3886627139529));
#18901=CARTESIAN_POINT('Ctrl Pts',(6.93160691706252,-3.3792984463582,5.49470538718602));
#18902=CARTESIAN_POINT('Ctrl Pts',(6.37115716117766,-3.00004224169406,5.58217557531111));
#18903=CARTESIAN_POINT('Ctrl Pts',(5.86067088430187,-2.98290615431278,5.6516158762443));
#18904=CARTESIAN_POINT('Ctrl Pts',(5.46137234532083,-3.12199756637258,5.70918062040184));
#18905=CARTESIAN_POINT('Ctrl Pts',(5.12579786574395,-3.44975370223118,5.77211265498338));
#18906=CARTESIAN_POINT('Ctrl Pts',(4.97675035295965,-3.93542942576474,5.84028080193706));
#18907=CARTESIAN_POINT('Ctrl Pts',(5.06033761012733,-4.34715442903143,5.89669313304848));
#18908=CARTESIAN_POINT('Ctrl Pts',(5.21589312480973,-4.58717538667364,5.93597358008697));
#18909=CARTESIAN_POINT('Ctrl Pts',(5.32753388253116,-4.70451276882046,5.95836231407345));
#18910=CARTESIAN_POINT('Ctrl Pts',(5.51520437334612,-4.85830387801752,5.9918868858073));
#18911=CARTESIAN_POINT('Ctrl Pts',(5.86247379692578,-4.99428552612942,6.0419557148591));
#18912=CARTESIAN_POINT('Ctrl Pts',(6.31174700962642,-4.93760907536453,6.10273651590458));
#18913=CARTESIAN_POINT('Ctrl Pts',(6.65339834000255,-4.72234495572188,6.15767095052905));
#18914=CARTESIAN_POINT('Ctrl Pts',(6.8679953212426,-4.43140295203578,6.20687048242351));
#18915=CARTESIAN_POINT('Ctrl Pts',(6.96101113211587,-4.08370529584463,6.25583653383823));
#18916=CARTESIAN_POINT('Ctrl Pts',(6.92075607352957,-3.72776957037704,6.30457519859578));
#18917=CARTESIAN_POINT('Ctrl Pts',(6.75390517552733,-3.41265101808349,6.35309493042986));
#18918=CARTESIAN_POINT('Ctrl Pts',(6.48475640607782,-3.18104900332911,6.40140514207317));
#18919=CARTESIAN_POINT('Ctrl Pts',(6.15098997417316,-3.06462900410609,6.44951457052472));
#18920=CARTESIAN_POINT('Ctrl Pts',(5.74035948083984,-3.0797743123596,6.50541569711097));
#18921=CARTESIAN_POINT('Ctrl Pts',(5.32224947191523,-3.31042394608842,6.5690097802638));
#18922=CARTESIAN_POINT('Ctrl Pts',(5.0641868258842,-3.77904585095687,6.64017852499677));
#18923=CARTESIAN_POINT('Ctrl Pts',(5.0893877649522,-4.22134632032621,6.6992024061301));
#18924=CARTESIAN_POINT('Ctrl Pts',(5.24761803700627,-4.52623489545367,6.74627803713346));
#18925=CARTESIAN_POINT('Ctrl Pts',(5.44354313111177,-4.73374792005069,6.78543039430136));
#18926=CARTESIAN_POINT('Ctrl Pts',(5.72295852635408,-4.88138222484995,6.82841428842587));
#18927=CARTESIAN_POINT('Ctrl Pts',(6.06447743648484,-4.91972128359138,6.87519838300688));
#18928=CARTESIAN_POINT('Ctrl Pts',(6.45152349101931,-4.81642569389462,6.92968667403752));
#18929=CARTESIAN_POINT('Ctrl Pts',(6.79954537293466,-4.50562749044762,6.99183260293409));
#18930=CARTESIAN_POINT('Ctrl Pts',(6.94448755821497,-4.00135704634088,7.06165092921972));
#18931=CARTESIAN_POINT('Ctrl Pts',(6.79951105295416,-3.49822641785881,7.13139191346124));
#18932=CARTESIAN_POINT('Ctrl Pts',(6.40903366533783,-3.14907814500179,7.20111945270289));
#18933=CARTESIAN_POINT('Ctrl Pts',(5.89262195791797,-3.06157288901472,7.27085739388313));
#18934=CARTESIAN_POINT('Ctrl Pts',(5.40812254199752,-3.26200851208852,7.34066372988413));
#18935=CARTESIAN_POINT('Ctrl Pts',(5.10418067172973,-3.69034738245555,7.41058819563509));
#18936=CARTESIAN_POINT('Ctrl Pts',(5.07421407730807,-4.21594541569564,7.48068129780375));
#18937=CARTESIAN_POINT('Ctrl Pts',(5.32958846913487,-4.67828762483568,7.55099734167383));
#18938=CARTESIAN_POINT('Ctrl Pts',(5.79329453600511,-4.93490538629606,7.62156008648381));
#18939=CARTESIAN_POINT('Ctrl Pts',(6.32466741939653,-4.90539161700316,7.69241833598134));
#18940=CARTESIAN_POINT('Ctrl Pts',(6.7611327378177,-4.59633338526078,7.763618222302));
#18941=CARTESIAN_POINT('Ctrl Pts',(6.96696593812447,-4.09977663923876,7.83517991770188));
#18942=CARTESIAN_POINT('Ctrl Pts',(6.87700234449016,-3.56684830698183,7.90714553328152));
#18943=CARTESIAN_POINT('Ctrl Pts',(6.51484228409451,-3.16087025594183,7.97956166490427));
#18944=CARTESIAN_POINT('Ctrl Pts',(5.98902418310519,-3.00899219730746,8.05244618048738));
#18945=CARTESIAN_POINT('Ctrl Pts',(5.45889377764469,-3.16073805954472,8.12584776997905));
#18946=CARTESIAN_POINT('Ctrl Pts',(5.10240229055434,-3.55916285129593,8.19702745975862));
#18947=CARTESIAN_POINT('Ctrl Pts',(5.00063529264588,-4.06258448759413,8.26596672294065));
#18948=CARTESIAN_POINT('Ctrl Pts',(5.14608638641085,-4.5370310753527,8.33258570888342));
#18949=CARTESIAN_POINT('Ctrl Pts',(5.47390473949641,-4.85700122338878,8.39407564739306));
#18950=CARTESIAN_POINT('Ctrl Pts',(5.86409370988404,-4.99349801167686,8.45031426874171));
#18951=CARTESIAN_POINT('Ctrl Pts',(6.23778180866483,-4.97982005074953,8.5012050843239));
#18952=CARTESIAN_POINT('Ctrl Pts',(6.5824024810436,-4.82957017385029,8.55235608559697));
#18953=CARTESIAN_POINT('Ctrl Pts',(6.84977764807081,-4.56249579195602,8.60378338768071));
#18954=CARTESIAN_POINT('Ctrl Pts',(7.0018975831038,-4.2143396128522,8.6554816689866));
#18955=CARTESIAN_POINT('Ctrl Pts',(7.01637606498482,-3.83268836849798,8.7074523074285));
#18956=CARTESIAN_POINT('Ctrl Pts',(6.88975870622095,-3.47023825895862,8.75969440257842));
#18957=CARTESIAN_POINT('Ctrl Pts',(6.63817267282148,-3.17759763612041,8.81220696108591));
#18958=CARTESIAN_POINT('Ctrl Pts',(6.29531438742434,-2.99617683490492,8.86498799953351));
#18959=CARTESIAN_POINT('Ctrl Pts',(5.90792353151983,-2.95234443557854,8.91803494390907));
#18960=CARTESIAN_POINT('Ctrl Pts',(5.52943465947779,-3.05356766071865,8.9713444776914));
#18961=CARTESIAN_POINT('Ctrl Pts',(5.21253830696404,-3.28722085945642,9.02491258570221));
#18962=CARTESIAN_POINT('Ctrl Pts',(5.00195199494555,-3.62204646733453,9.07873463013611));
#18963=CARTESIAN_POINT('Ctrl Pts',(4.92781914311232,-4.01254248071306,9.13280515564705));
#18964=CARTESIAN_POINT('Ctrl Pts',(5.00199615651236,-4.40470108927855,9.18711842200491));
#18965=CARTESIAN_POINT('Ctrl Pts',(5.23867881713171,-4.78221302009702,9.24772886990218));
#18966=CARTESIAN_POINT('Ctrl Pts',(5.65754135413719,-5.05347587134047,9.31472611241896));
#18967=CARTESIAN_POINT('Ctrl Pts',(6.20369084805172,-5.09446619773149,9.38820047058106));
#18968=CARTESIAN_POINT('Ctrl Pts',(6.58491140028356,-4.9227463833809,9.44435213091082));
#18969=CARTESIAN_POINT('Ctrl Pts',(6.79043706915131,-4.73349491889994,9.48292799960354));
#18970=CARTESIAN_POINT('Ctrl Pts',(6.91812074774067,-4.57790769275921,9.51073873753964));
#18971=CARTESIAN_POINT('Ctrl Pts',(7.08206628048093,-4.26214523314509,9.55949576991338));
#18972=CARTESIAN_POINT('Ctrl Pts',(7.11203000974648,-3.73801507749313,9.62940143023879));
#18973=CARTESIAN_POINT('Ctrl Pts',(6.80607956694539,-3.18372878894946,9.71365355088675));
#18974=CARTESIAN_POINT('Ctrl Pts',(6.2500729387616,-2.87606410279642,9.79823196594816));
#18975=CARTESIAN_POINT('Ctrl Pts',(5.61350827590933,-2.91164276328602,9.88309878900258));
#18976=CARTESIAN_POINT('Ctrl Pts',(5.09167653337187,-3.28121508261429,9.96820541651057));
#18977=CARTESIAN_POINT('Ctrl Pts',(4.84631772029848,-3.87343097145342,10.053501888748));
#18978=CARTESIAN_POINT('Ctrl Pts',(4.95370265231542,-4.50645428090226,10.1389580152242));
#18979=CARTESIAN_POINT('Ctrl Pts',(5.38206584333841,-4.98594004162619,10.224520377509));
#18980=CARTESIAN_POINT('Ctrl Pts',(6.00029102821274,-5.16409124961399,10.310145146497));
#18981=CARTESIAN_POINT('Ctrl Pts',(6.61864143146891,-4.9859514705061,10.395783712958));
#18982=CARTESIAN_POINT('Ctrl Pts',(7.04722318405374,-4.50628003310617,10.4813893153194));
#18983=CARTESIAN_POINT('Ctrl Pts',(7.15476578245007,-3.87269332662491,10.5669147992673));
#18984=CARTESIAN_POINT('Ctrl Pts',(6.90903852094291,-3.27989871424364,10.6523132378576));
#18985=CARTESIAN_POINT('Ctrl Pts',(6.38662842519509,-2.909479749711,10.7375396128794));
#18986=CARTESIAN_POINT('Ctrl Pts',(5.7487891451485,-2.87392013799551,10.8225468482879));
#18987=CARTESIAN_POINT('Ctrl Pts',(5.19161128486125,-3.18222383349236,10.9072959154668));
#18988=CARTESIAN_POINT('Ctrl Pts',(4.88477218880103,-3.7377854487073,10.991733743207));
#18989=CARTESIAN_POINT('Ctrl Pts',(4.92090890603324,-4.36871687716726,11.0758429802562));
#18990=CARTESIAN_POINT('Ctrl Pts',(5.28513006682729,-4.8816390523311,11.1595745791957));
#18991=CARTESIAN_POINT('Ctrl Pts',(5.86367097478207,-5.12070465769319,11.2428883860081));
#18992=CARTESIAN_POINT('Ctrl Pts',(6.47730091809014,-5.01618325405715,11.3257454113017));
#18993=CARTESIAN_POINT('Ctrl Pts',(6.93846782961665,-4.60290035590192,11.4081371563723));
#18994=CARTESIAN_POINT('Ctrl Pts',(7.05150181122088,-4.20962129145193,11.4626969504376));
#18995=CARTESIAN_POINT('Ctrl Pts',(7.05152835862385,-4.01242066548927,11.4899208404075));
#18996=CARTESIAN_POINT('Ctrl Pts',(6.99999815899365,-3.98632452652653,2.60093950625054));
#18997=CARTESIAN_POINT('Ctrl Pts',(6.99997288064459,-3.79855038269031,2.62686205390176));
#18998=CARTESIAN_POINT('Ctrl Pts',(6.89233514047511,-3.42414397295474,2.67881370715146));
#18999=CARTESIAN_POINT('Ctrl Pts',(6.45271448161715,-3.02998089899105,2.757384351524));
#19000=CARTESIAN_POINT('Ctrl Pts',(5.86671979479608,-2.93006055988124,2.83651312593273));
#19001=CARTESIAN_POINT('Ctrl Pts',(5.31329781017118,-3.15858496371257,2.91622300969429));
#19002=CARTESIAN_POINT('Ctrl Pts',(4.9638387202763,-3.65012742948249,2.99648818069946));
#19003=CARTESIAN_POINT('Ctrl Pts',(4.9293710419426,-4.25616717719541,3.07729927110974));
#19004=CARTESIAN_POINT('Ctrl Pts',(5.22419213535424,-4.79140012919127,3.15863486906283));
#19005=CARTESIAN_POINT('Ctrl Pts',(5.76222069265107,-5.08919945404236,3.24047453667969));
#19006=CARTESIAN_POINT('Ctrl Pts',(6.379677030618,-5.05504702300603,3.32279319426342));
#19007=CARTESIAN_POINT('Ctrl Pts',(6.88712884688249,-4.6955749219134,3.40556355651458));
#19008=CARTESIAN_POINT('Ctrl Pts',(7.12670085302573,-4.11831918936923,3.48875539197247));
#19009=CARTESIAN_POINT('Ctrl Pts',(7.02192637673817,-3.49920475943206,3.57233609217612));
#19010=CARTESIAN_POINT('Ctrl Pts',(6.60200480535371,-3.02877356919622,3.65627071403784));
#19011=CARTESIAN_POINT('Ctrl Pts',(5.99389696970595,-2.85326346917548,3.74052223770667));
#19012=CARTESIAN_POINT('Ctrl Pts',(5.38356210524816,-3.02876561374954,3.82505176545516));
#19013=CARTESIAN_POINT('Ctrl Pts',(4.97486808401256,-3.48597581907603,3.90667922332894));
#19014=CARTESIAN_POINT('Ctrl Pts',(4.87764331063032,-3.96854834063101,3.97275270796177));
#19015=CARTESIAN_POINT('Ctrl Pts',(4.93363491104256,-4.28466096216571,4.01685604464165));
#19016=CARTESIAN_POINT('Ctrl Pts',(4.99817931143911,-4.45530970670709,4.04207155735716));
#19017=CARTESIAN_POINT('Ctrl Pts',(5.12597275373369,-4.69744865131441,4.07990746653167));
#19018=CARTESIAN_POINT('Ctrl Pts',(5.42875069944469,-4.99309340796393,4.13670511444809));
#19019=CARTESIAN_POINT('Ctrl Pts',(5.97231920216535,-5.14605898976926,4.21249748606625));
#19020=CARTESIAN_POINT('Ctrl Pts',(6.52320508223107,-5.02044374257342,4.28832048254892));
#19021=CARTESIAN_POINT('Ctrl Pts',(6.91110467076896,-4.67743260856581,4.35782392841035));
#19022=CARTESIAN_POINT('Ctrl Pts',(7.09644745188598,-4.25185787791867,4.42098501720712));
#19023=CARTESIAN_POINT('Ctrl Pts',(7.11227598252982,-3.83457932502243,4.47779828333078));
#19024=CARTESIAN_POINT('Ctrl Pts',(6.97422198867159,-3.44096105119827,4.53456659991209));
#19025=CARTESIAN_POINT('Ctrl Pts',(6.67241777459347,-3.08955752755044,4.59757801617794));
#19026=CARTESIAN_POINT('Ctrl Pts',(6.20242890124212,-2.8776477149725,4.66678930738527));
#19027=CARTESIAN_POINT('Ctrl Pts',(5.64251878205079,-2.91980762281901,4.74213608937642));
#19028=CARTESIAN_POINT('Ctrl Pts',(5.2704159386044,-3.1605530148329,4.80163845364204));
#19029=CARTESIAN_POINT('Ctrl Pts',(5.0774166278585,-3.41255654376288,4.84539629257686));
#19030=CARTESIAN_POINT('Ctrl Pts',(4.95479769651029,-3.65506677262475,4.88286085266752));
#19031=CARTESIAN_POINT('Ctrl Pts',(4.89096164216428,-3.99267527518354,4.9296088561907));
#19032=CARTESIAN_POINT('Ctrl Pts',(4.9676452372308,-4.39667000889553,4.98556279567646));
#19033=CARTESIAN_POINT('Ctrl Pts',(5.18583996189851,-4.74396038265063,5.04136211338706));
#19034=CARTESIAN_POINT('Ctrl Pts',(5.51489715544512,-4.98648283834255,5.09699623582978));
#19035=CARTESIAN_POINT('Ctrl Pts',(5.90877797642046,-5.0921366099034,5.15245506500268));
#19036=CARTESIAN_POINT('Ctrl Pts',(6.31208382647452,-5.04618505638536,5.20772889790527));
#19037=CARTESIAN_POINT('Ctrl Pts',(6.79039563711824,-4.79482787477752,5.28116853494519));
#19038=CARTESIAN_POINT('Ctrl Pts',(7.14364250607538,-4.18339760328549,5.37246079320281));
#19039=CARTESIAN_POINT('Ctrl Pts',(6.95465392442801,-3.3615290602033,5.48113680479085));
#19040=CARTESIAN_POINT('Ctrl Pts',(6.37954281770185,-2.97211167108618,5.57092649504958));
#19041=CARTESIAN_POINT('Ctrl Pts',(5.85508217241069,-2.95446460563552,5.64227218334414));
#19042=CARTESIAN_POINT('Ctrl Pts',(5.44460306454923,-3.0974244576334,5.70145206942602));
#19043=CARTESIAN_POINT('Ctrl Pts',(5.09938139322235,-3.43453521092238,5.76619150122483));
#19044=CARTESIAN_POINT('Ctrl Pts',(4.94592320318296,-3.93442474869926,5.83636208316637));
#19045=CARTESIAN_POINT('Ctrl Pts',(5.03197265676116,-4.35840627465708,5.89445465107149));
#19046=CARTESIAN_POINT('Ctrl Pts',(5.19219264369348,-4.60564299044654,5.93491706685731));
#19047=CARTESIAN_POINT('Ctrl Pts',(5.30719577297855,-4.72651611720447,5.95798055540973));
#19048=CARTESIAN_POINT('Ctrl Pts',(5.50053046023923,-4.88495348501329,5.99251787759586));
#19049=CARTESIAN_POINT('Ctrl Pts',(5.85832951556707,-5.02507253962729,6.04410658286047));
#19050=CARTESIAN_POINT('Ctrl Pts',(6.32126493019694,-4.96668267597821,6.10673564915363));
#19051=CARTESIAN_POINT('Ctrl Pts',(6.67328517320073,-4.74489735077078,6.1633365491453));
#19052=CARTESIAN_POINT('Ctrl Pts',(6.89435900913716,-4.44516759248262,6.21402149084589));
#19053=CARTESIAN_POINT('Ctrl Pts',(6.99016055458223,-4.08705298460299,6.26445344730346));
#19054=CARTESIAN_POINT('Ctrl Pts',(6.94870527391535,-3.72056310115263,6.31463598339954));
#19055=CARTESIAN_POINT('Ctrl Pts',(6.77696548585144,-3.39623351183634,6.36457330966794));
#19056=CARTESIAN_POINT('Ctrl Pts',(6.50006848678236,-3.15797695360399,6.41427030439494));
#19057=CARTESIAN_POINT('Ctrl Pts',(6.15689079921747,-3.03828948600061,6.46373243937456));
#19058=CARTESIAN_POINT('Ctrl Pts',(5.73494713487383,-3.05387392617641,6.52117143017342));
#19059=CARTESIAN_POINT('Ctrl Pts',(5.30575107583077,-3.29070893773119,6.58644590514151));
#19060=CARTESIAN_POINT('Ctrl Pts',(5.04125313845857,-3.77122732190886,6.6594050878354));
#19061=CARTESIAN_POINT('Ctrl Pts',(5.06714113786846,-4.2240700226978,6.71983222627245));
#19062=CARTESIAN_POINT('Ctrl Pts',(5.22896371026909,-4.53583531846688,6.76796591127916));
#19063=CARTESIAN_POINT('Ctrl Pts',(5.42916113979845,-4.74785467675554,6.80796630808184));
#19064=CARTESIAN_POINT('Ctrl Pts',(5.714367370309,-4.89850759732021,6.85183024025803));
#19065=CARTESIAN_POINT('Ctrl Pts',(6.06253639457921,-4.93755475445945,6.89952195690528));
#19066=CARTESIAN_POINT('Ctrl Pts',(6.4565847787629,-4.83233977440753,6.95498839066731));
#19067=CARTESIAN_POINT('Ctrl Pts',(6.81022730237302,-4.51633849133825,7.01814871600544));
#19068=CARTESIAN_POINT('Ctrl Pts',(6.95706828830077,-4.00489886911992,7.08893287981098));
#19069=CARTESIAN_POINT('Ctrl Pts',(6.81021224891959,-3.49584469103884,7.15948666255227));
#19070=CARTESIAN_POINT('Ctrl Pts',(6.41592301667082,-3.14352189275395,7.22985222727915));
#19071=CARTESIAN_POINT('Ctrl Pts',(5.89582428767248,-3.0555832223308,7.30007283378182));
#19072=CARTESIAN_POINT('Ctrl Pts',(5.40914881608276,-3.25711226719962,7.37019262219717));
#19073=CARTESIAN_POINT('Ctrl Pts',(5.10471600640629,-3.68647088534127,7.4402563254545));
#19074=CARTESIAN_POINT('Ctrl Pts',(5.07493689936822,-4.21187381141773,7.51030900528994));
#19075=CARTESIAN_POINT('Ctrl Pts',(5.32972438815395,-4.67276168571651,7.58039577687912));
#19076=CARTESIAN_POINT('Ctrl Pts',(5.79102554371443,-4.92784792737786,7.65056157421906));
#19077=CARTESIAN_POINT('Ctrl Pts',(6.31826031255578,-4.89837953861158,7.72085085714204));
#19078=CARTESIAN_POINT('Ctrl Pts',(6.75020660471299,-4.59231290695902,7.79130734550421));
#19079=CARTESIAN_POINT('Ctrl Pts',(6.95334524231267,-4.10180979072915,7.86197377515194));
#19080=CARTESIAN_POINT('Ctrl Pts',(6.86452811856373,-3.57660445666216,7.93289164673106));
#19081=CARTESIAN_POINT('Ctrl Pts',(6.50822949801913,-3.17741851765368,8.00410096472273));
#19082=CARTESIAN_POINT('Ctrl Pts',(5.99202912111436,-3.02846879700038,8.07564001126929));
#19083=CARTESIAN_POINT('Ctrl Pts',(5.47262775862424,-3.1772786287127,8.14754510192845));
#19084=CARTESIAN_POINT('Ctrl Pts',(5.12396773984527,-3.56713104102442,8.21717245978697));
#19085=CARTESIAN_POINT('Ctrl Pts',(5.02465088008016,-4.0589090579052,8.28449962671212));
#19086=CARTESIAN_POINT('Ctrl Pts',(5.16664179671633,-4.52183049710153,8.34949563002517));
#19087=CARTESIAN_POINT('Ctrl Pts',(5.48622133819085,-4.83366725020512,8.40942447534479));
#19088=CARTESIAN_POINT('Ctrl Pts',(5.86625745021743,-4.9665851067969,8.4641954747342));
#19089=CARTESIAN_POINT('Ctrl Pts',(6.22997586892847,-4.95324406413884,8.5137197914407));
#19090=CARTESIAN_POINT('Ctrl Pts',(6.56523678307791,-4.80705258085916,8.56348049146453));
#19091=CARTESIAN_POINT('Ctrl Pts',(6.8252178463785,-4.54733568382595,8.61348288991823));
#19092=CARTESIAN_POINT('Ctrl Pts',(6.97306928054101,-4.20890471076454,8.6637316832973));
#19093=CARTESIAN_POINT('Ctrl Pts',(6.98712341108126,-3.83802816814003,8.7142309149468));
#19094=CARTESIAN_POINT('Ctrl Pts',(6.86409431800442,-3.4858887373625,8.76498396878373));
#19095=CARTESIAN_POINT('Ctrl Pts',(6.61968641501593,-3.20161333099039,8.81599356080702));
#19096=CARTESIAN_POINT('Ctrl Pts',(6.28663539552411,-3.02539046352671,8.8672617337013));
#19097=CARTESIAN_POINT('Ctrl Pts',(5.91032079687008,-2.98281618785264,8.9187898484193));
#19098=CARTESIAN_POINT('Ctrl Pts',(5.54261902100133,-3.08115683102349,8.97057858319571));
#19099=CARTESIAN_POINT('Ctrl Pts',(5.23470149593991,-3.30818973404657,9.02262792887906));
#19100=CARTESIAN_POINT('Ctrl Pts',(5.03002953653242,-3.63360637314209,9.07493719454492));
#19101=CARTESIAN_POINT('Ctrl Pts',(4.95795339049146,-4.01324887545392,9.12750499722226));
#19102=CARTESIAN_POINT('Ctrl Pts',(5.03008733681497,-4.39465616925505,9.18032929191999));
#19103=CARTESIAN_POINT('Ctrl Pts',(5.26037098227884,-4.76198737973904,9.23930488376548));
#19104=CARTESIAN_POINT('Ctrl Pts',(5.66815402132354,-5.02611715334513,9.30453505328307));
#19105=CARTESIAN_POINT('Ctrl Pts',(6.20031175950905,-5.06610553161693,9.37613052247429));
#19106=CARTESIAN_POINT('Ctrl Pts',(6.57211483447548,-4.89867154701958,9.43089482659667));
#19107=CARTESIAN_POINT('Ctrl Pts',(6.77268428325753,-4.71398594666241,9.46854124254023));
#19108=CARTESIAN_POINT('Ctrl Pts',(6.89732261541234,-4.56210906285714,9.4956893772699));
#19109=CARTESIAN_POINT('Ctrl Pts',(7.05743952416135,-4.25373892219051,9.54330952558428));
#19110=CARTESIAN_POINT('Ctrl Pts',(7.08681427060224,-3.7413976498585,9.61164803498953));
#19111=CARTESIAN_POINT('Ctrl Pts',(6.78743967682059,-3.19877575055479,9.69412425474241));
#19112=CARTESIAN_POINT('Ctrl Pts',(6.24245837315985,-2.89706443193603,9.77704206668623));
#19113=CARTESIAN_POINT('Ctrl Pts',(5.61746900273164,-2.93185417099466,9.86037047868398));
#19114=CARTESIAN_POINT('Ctrl Pts',(5.1042042416184,-3.29518411512121,9.94407604361117));
#19115=CARTESIAN_POINT('Ctrl Pts',(4.86233946758306,-3.8785536270643,10.0281231251224));
#19116=CARTESIAN_POINT('Ctrl Pts',(4.96816269898698,-4.50332086698013,10.1124740074888));
#19117=CARTESIAN_POINT('Ctrl Pts',(5.3915816199262,-4.97752738430232,10.1970892227568));
#19118=CARTESIAN_POINT('Ctrl Pts',(6.00397807691952,-5.15417755509278,10.281927720062));
#19119=CARTESIAN_POINT('Ctrl Pts',(6.61779621608409,-4.97752665860305,10.3669471357688));
#19120=CARTESIAN_POINT('Ctrl Pts',(7.04418758947222,-4.50057596349951,10.4521040140405));
#19121=CARTESIAN_POINT('Ctrl Pts',(7.15154318711507,-3.86917823804319,10.5373541207604));
#19122=CARTESIAN_POINT('Ctrl Pts',(6.9063217242137,-3.27712490715728,10.622652644332));
#19123=CARTESIAN_POINT('Ctrl Pts',(6.38365961018741,-2.90630232377856,10.70795449752));
#19124=CARTESIAN_POINT('Ctrl Pts',(5.74407957751689,-2.87046702674317,10.7932145497474));
#19125=CARTESIAN_POINT('Ctrl Pts',(5.18413779010185,-3.18009512220889,10.8783879953558));
#19126=CARTESIAN_POINT('Ctrl Pts',(4.87504525063398,-3.73939474085648,10.9634303821887));
#19127=CARTESIAN_POINT('Ctrl Pts',(4.9113280193628,-4.37593360867611,11.0482983399598));
#19128=CARTESIAN_POINT('Ctrl Pts',(5.27937248430205,-4.89450749674953,11.1329488708158));
#19129=CARTESIAN_POINT('Ctrl Pts',(5.86527624347711,-5.13679808752952,11.2173417295453));
#19130=CARTESIAN_POINT('Ctrl Pts',(6.48799534199112,-5.03087191620999,11.3014349903219));
#19131=CARTESIAN_POINT('Ctrl Pts',(6.95693136473707,-4.61090781293032,11.3851957485584));
#19132=CARTESIAN_POINT('Ctrl Pts',(7.07219562678886,-4.21035033769926,11.4407823887657));
#19133=CARTESIAN_POINT('Ctrl Pts',(7.07222266979228,-4.00946826992833,11.4685145081909));
#19134=CARTESIAN_POINT('',(6.99999815899365,-3.98632452652653,2.60093950625054));
#19135=CARTESIAN_POINT('Origin',(7.,-4.,2.7));
#19136=CARTESIAN_POINT('',(7.07222266979228,-4.00946826992833,11.4685145081909));
#19137=CARTESIAN_POINT('Ctrl Pts',(6.99999815899365,-3.98632452652653,2.60093950625054));
#19138=CARTESIAN_POINT('Ctrl Pts',(6.99997288064459,-3.79855038269031,2.62686205390176));
#19139=CARTESIAN_POINT('Ctrl Pts',(6.89233514047511,-3.42414397295474,2.67881370715146));
#19140=CARTESIAN_POINT('Ctrl Pts',(6.45271448161715,-3.02998089899105,2.757384351524));
#19141=CARTESIAN_POINT('Ctrl Pts',(5.86671979479608,-2.93006055988124,2.83651312593273));
#19142=CARTESIAN_POINT('Ctrl Pts',(5.31329781017118,-3.15858496371257,2.91622300969429));
#19143=CARTESIAN_POINT('Ctrl Pts',(4.9638387202763,-3.65012742948249,2.99648818069946));
#19144=CARTESIAN_POINT('Ctrl Pts',(4.9293710419426,-4.25616717719541,3.07729927110974));
#19145=CARTESIAN_POINT('Ctrl Pts',(5.22419213535424,-4.79140012919127,3.15863486906283));
#19146=CARTESIAN_POINT('Ctrl Pts',(5.76222069265107,-5.08919945404236,3.24047453667969));
#19147=CARTESIAN_POINT('Ctrl Pts',(6.379677030618,-5.05504702300603,3.32279319426342));
#19148=CARTESIAN_POINT('Ctrl Pts',(6.88712884688249,-4.6955749219134,3.40556355651458));
#19149=CARTESIAN_POINT('Ctrl Pts',(7.12670085302573,-4.11831918936923,3.48875539197247));
#19150=CARTESIAN_POINT('Ctrl Pts',(7.02192637673817,-3.49920475943206,3.57233609217612));
#19151=CARTESIAN_POINT('Ctrl Pts',(6.60200480535371,-3.02877356919622,3.65627071403784));
#19152=CARTESIAN_POINT('Ctrl Pts',(5.99389696970595,-2.85326346917548,3.74052223770667));
#19153=CARTESIAN_POINT('Ctrl Pts',(5.38356210524816,-3.02876561374954,3.82505176545516));
#19154=CARTESIAN_POINT('Ctrl Pts',(4.97486808401256,-3.48597581907603,3.90667922332894));
#19155=CARTESIAN_POINT('Ctrl Pts',(4.87764331063032,-3.96854834063101,3.97275270796177));
#19156=CARTESIAN_POINT('Ctrl Pts',(4.93363491104256,-4.28466096216571,4.01685604464165));
#19157=CARTESIAN_POINT('Ctrl Pts',(4.99817931143911,-4.45530970670709,4.04207155735716));
#19158=CARTESIAN_POINT('Ctrl Pts',(5.12597275373369,-4.69744865131441,4.07990746653167));
#19159=CARTESIAN_POINT('Ctrl Pts',(5.42875069944469,-4.99309340796393,4.13670511444809));
#19160=CARTESIAN_POINT('Ctrl Pts',(5.97231920216535,-5.14605898976926,4.21249748606625));
#19161=CARTESIAN_POINT('Ctrl Pts',(6.52320508223107,-5.02044374257342,4.28832048254892));
#19162=CARTESIAN_POINT('Ctrl Pts',(6.91110467076896,-4.67743260856581,4.35782392841035));
#19163=CARTESIAN_POINT('Ctrl Pts',(7.09644745188598,-4.25185787791867,4.42098501720712));
#19164=CARTESIAN_POINT('Ctrl Pts',(7.11227598252982,-3.83457932502243,4.47779828333078));
#19165=CARTESIAN_POINT('Ctrl Pts',(6.97422198867159,-3.44096105119827,4.53456659991209));
#19166=CARTESIAN_POINT('Ctrl Pts',(6.67241777459347,-3.08955752755044,4.59757801617794));
#19167=CARTESIAN_POINT('Ctrl Pts',(6.20242890124212,-2.8776477149725,4.66678930738527));
#19168=CARTESIAN_POINT('Ctrl Pts',(5.64251878205079,-2.91980762281901,4.74213608937642));
#19169=CARTESIAN_POINT('Ctrl Pts',(5.2704159386044,-3.1605530148329,4.80163845364204));
#19170=CARTESIAN_POINT('Ctrl Pts',(5.0774166278585,-3.41255654376288,4.84539629257686));
#19171=CARTESIAN_POINT('Ctrl Pts',(4.95479769651029,-3.65506677262475,4.88286085266752));
#19172=CARTESIAN_POINT('Ctrl Pts',(4.89096164216428,-3.99267527518354,4.9296088561907));
#19173=CARTESIAN_POINT('Ctrl Pts',(4.9676452372308,-4.39667000889553,4.98556279567646));
#19174=CARTESIAN_POINT('Ctrl Pts',(5.18583996189851,-4.74396038265063,5.04136211338706));
#19175=CARTESIAN_POINT('Ctrl Pts',(5.51489715544512,-4.98648283834255,5.09699623582978));
#19176=CARTESIAN_POINT('Ctrl Pts',(5.90877797642046,-5.0921366099034,5.15245506500268));
#19177=CARTESIAN_POINT('Ctrl Pts',(6.31208382647452,-5.04618505638536,5.20772889790527));
#19178=CARTESIAN_POINT('Ctrl Pts',(6.79039563711824,-4.79482787477752,5.28116853494519));
#19179=CARTESIAN_POINT('Ctrl Pts',(7.14364250607538,-4.18339760328549,5.37246079320281));
#19180=CARTESIAN_POINT('Ctrl Pts',(6.95465392442801,-3.3615290602033,5.48113680479085));
#19181=CARTESIAN_POINT('Ctrl Pts',(6.37954281770185,-2.97211167108618,5.57092649504958));
#19182=CARTESIAN_POINT('Ctrl Pts',(5.85508217241069,-2.95446460563552,5.64227218334414));
#19183=CARTESIAN_POINT('Ctrl Pts',(5.44460306454923,-3.0974244576334,5.70145206942602));
#19184=CARTESIAN_POINT('Ctrl Pts',(5.09938139322235,-3.43453521092238,5.76619150122483));
#19185=CARTESIAN_POINT('Ctrl Pts',(4.94592320318296,-3.93442474869926,5.83636208316637));
#19186=CARTESIAN_POINT('Ctrl Pts',(5.03197265676116,-4.35840627465708,5.89445465107149));
#19187=CARTESIAN_POINT('Ctrl Pts',(5.19219264369348,-4.60564299044654,5.93491706685731));
#19188=CARTESIAN_POINT('Ctrl Pts',(5.30719577297855,-4.72651611720447,5.95798055540973));
#19189=CARTESIAN_POINT('Ctrl Pts',(5.50053046023923,-4.88495348501329,5.99251787759586));
#19190=CARTESIAN_POINT('Ctrl Pts',(5.85832951556707,-5.02507253962729,6.04410658286047));
#19191=CARTESIAN_POINT('Ctrl Pts',(6.32126493019694,-4.96668267597821,6.10673564915363));
#19192=CARTESIAN_POINT('Ctrl Pts',(6.67328517320073,-4.74489735077078,6.1633365491453));
#19193=CARTESIAN_POINT('Ctrl Pts',(6.89435900913716,-4.44516759248262,6.21402149084589));
#19194=CARTESIAN_POINT('Ctrl Pts',(6.99016055458223,-4.08705298460299,6.26445344730346));
#19195=CARTESIAN_POINT('Ctrl Pts',(6.94870527391535,-3.72056310115263,6.31463598339954));
#19196=CARTESIAN_POINT('Ctrl Pts',(6.77696548585144,-3.39623351183634,6.36457330966794));
#19197=CARTESIAN_POINT('Ctrl Pts',(6.50006848678236,-3.15797695360399,6.41427030439494));
#19198=CARTESIAN_POINT('Ctrl Pts',(6.15689079921747,-3.03828948600061,6.46373243937456));
#19199=CARTESIAN_POINT('Ctrl Pts',(5.73494713487383,-3.05387392617641,6.52117143017342));
#19200=CARTESIAN_POINT('Ctrl Pts',(5.30575107583077,-3.29070893773119,6.58644590514151));
#19201=CARTESIAN_POINT('Ctrl Pts',(5.04125313845857,-3.77122732190886,6.6594050878354));
#19202=CARTESIAN_POINT('Ctrl Pts',(5.06714113786846,-4.2240700226978,6.71983222627245));
#19203=CARTESIAN_POINT('Ctrl Pts',(5.22896371026909,-4.53583531846688,6.76796591127916));
#19204=CARTESIAN_POINT('Ctrl Pts',(5.42916113979845,-4.74785467675554,6.80796630808184));
#19205=CARTESIAN_POINT('Ctrl Pts',(5.714367370309,-4.89850759732021,6.85183024025803));
#19206=CARTESIAN_POINT('Ctrl Pts',(6.06253639457921,-4.93755475445945,6.89952195690528));
#19207=CARTESIAN_POINT('Ctrl Pts',(6.4565847787629,-4.83233977440753,6.95498839066731));
#19208=CARTESIAN_POINT('Ctrl Pts',(6.81022730237302,-4.51633849133825,7.01814871600544));
#19209=CARTESIAN_POINT('Ctrl Pts',(6.95706828830077,-4.00489886911992,7.08893287981098));
#19210=CARTESIAN_POINT('Ctrl Pts',(6.81021224891959,-3.49584469103884,7.15948666255227));
#19211=CARTESIAN_POINT('Ctrl Pts',(6.41592301667082,-3.14352189275395,7.22985222727915));
#19212=CARTESIAN_POINT('Ctrl Pts',(5.89582428767248,-3.0555832223308,7.30007283378182));
#19213=CARTESIAN_POINT('Ctrl Pts',(5.40914881608276,-3.25711226719962,7.37019262219717));
#19214=CARTESIAN_POINT('Ctrl Pts',(5.10471600640629,-3.68647088534127,7.4402563254545));
#19215=CARTESIAN_POINT('Ctrl Pts',(5.07493689936822,-4.21187381141773,7.51030900528994));
#19216=CARTESIAN_POINT('Ctrl Pts',(5.32972438815395,-4.67276168571651,7.58039577687912));
#19217=CARTESIAN_POINT('Ctrl Pts',(5.79102554371443,-4.92784792737786,7.65056157421906));
#19218=CARTESIAN_POINT('Ctrl Pts',(6.31826031255578,-4.89837953861158,7.72085085714204));
#19219=CARTESIAN_POINT('Ctrl Pts',(6.75020660471299,-4.59231290695902,7.79130734550421));
#19220=CARTESIAN_POINT('Ctrl Pts',(6.95334524231267,-4.10180979072915,7.86197377515194));
#19221=CARTESIAN_POINT('Ctrl Pts',(6.86452811856373,-3.57660445666216,7.93289164673106));
#19222=CARTESIAN_POINT('Ctrl Pts',(6.50822949801913,-3.17741851765368,8.00410096472273));
#19223=CARTESIAN_POINT('Ctrl Pts',(5.99202912111436,-3.02846879700038,8.07564001126929));
#19224=CARTESIAN_POINT('Ctrl Pts',(5.47262775862424,-3.1772786287127,8.14754510192845));
#19225=CARTESIAN_POINT('Ctrl Pts',(5.12396773984527,-3.56713104102442,8.21717245978697));
#19226=CARTESIAN_POINT('Ctrl Pts',(5.02465088008016,-4.0589090579052,8.28449962671212));
#19227=CARTESIAN_POINT('Ctrl Pts',(5.16664179671633,-4.52183049710153,8.34949563002517));
#19228=CARTESIAN_POINT('Ctrl Pts',(5.48622133819085,-4.83366725020512,8.40942447534479));
#19229=CARTESIAN_POINT('Ctrl Pts',(5.86625745021743,-4.9665851067969,8.4641954747342));
#19230=CARTESIAN_POINT('Ctrl Pts',(6.22997586892847,-4.95324406413884,8.5137197914407));
#19231=CARTESIAN_POINT('Ctrl Pts',(6.56523678307791,-4.80705258085916,8.56348049146453));
#19232=CARTESIAN_POINT('Ctrl Pts',(6.8252178463785,-4.54733568382595,8.61348288991823));
#19233=CARTESIAN_POINT('Ctrl Pts',(6.97306928054101,-4.20890471076454,8.6637316832973));
#19234=CARTESIAN_POINT('Ctrl Pts',(6.98712341108126,-3.83802816814003,8.7142309149468));
#19235=CARTESIAN_POINT('Ctrl Pts',(6.86409431800442,-3.4858887373625,8.76498396878373));
#19236=CARTESIAN_POINT('Ctrl Pts',(6.61968641501593,-3.20161333099039,8.81599356080702));
#19237=CARTESIAN_POINT('Ctrl Pts',(6.28663539552411,-3.02539046352671,8.8672617337013));
#19238=CARTESIAN_POINT('Ctrl Pts',(5.91032079687008,-2.98281618785264,8.9187898484193));
#19239=CARTESIAN_POINT('Ctrl Pts',(5.54261902100133,-3.08115683102349,8.97057858319571));
#19240=CARTESIAN_POINT('Ctrl Pts',(5.23470149593991,-3.30818973404657,9.02262792887906));
#19241=CARTESIAN_POINT('Ctrl Pts',(5.03002953653242,-3.63360637314209,9.07493719454492));
#19242=CARTESIAN_POINT('Ctrl Pts',(4.95795339049146,-4.01324887545392,9.12750499722226));
#19243=CARTESIAN_POINT('Ctrl Pts',(5.03008733681497,-4.39465616925505,9.18032929191999));
#19244=CARTESIAN_POINT('Ctrl Pts',(5.26037098227884,-4.76198737973904,9.23930488376548));
#19245=CARTESIAN_POINT('Ctrl Pts',(5.66815402132354,-5.02611715334513,9.30453505328307));
#19246=CARTESIAN_POINT('Ctrl Pts',(6.20031175950905,-5.06610553161693,9.37613052247429));
#19247=CARTESIAN_POINT('Ctrl Pts',(6.57211483447548,-4.89867154701958,9.43089482659667));
#19248=CARTESIAN_POINT('Ctrl Pts',(6.77268428325753,-4.71398594666241,9.46854124254023));
#19249=CARTESIAN_POINT('Ctrl Pts',(6.89732261541234,-4.56210906285714,9.4956893772699));
#19250=CARTESIAN_POINT('Ctrl Pts',(7.05743952416135,-4.25373892219051,9.54330952558428));
#19251=CARTESIAN_POINT('Ctrl Pts',(7.08681427060224,-3.7413976498585,9.61164803498953));
#19252=CARTESIAN_POINT('Ctrl Pts',(6.78743967682059,-3.19877575055479,9.69412425474241));
#19253=CARTESIAN_POINT('Ctrl Pts',(6.24245837315985,-2.89706443193603,9.77704206668623));
#19254=CARTESIAN_POINT('Ctrl Pts',(5.61746900273164,-2.93185417099466,9.86037047868398));
#19255=CARTESIAN_POINT('Ctrl Pts',(5.1042042416184,-3.29518411512121,9.94407604361117));
#19256=CARTESIAN_POINT('Ctrl Pts',(4.86233946758306,-3.8785536270643,10.0281231251224));
#19257=CARTESIAN_POINT('Ctrl Pts',(4.96816269898698,-4.50332086698013,10.1124740074888));
#19258=CARTESIAN_POINT('Ctrl Pts',(5.3915816199262,-4.97752738430232,10.1970892227568));
#19259=CARTESIAN_POINT('Ctrl Pts',(6.00397807691952,-5.15417755509278,10.281927720062));
#19260=CARTESIAN_POINT('Ctrl Pts',(6.61779621608409,-4.97752665860305,10.3669471357688));
#19261=CARTESIAN_POINT('Ctrl Pts',(7.04418758947222,-4.50057596349951,10.4521040140405));
#19262=CARTESIAN_POINT('Ctrl Pts',(7.15154318711507,-3.86917823804319,10.5373541207604));
#19263=CARTESIAN_POINT('Ctrl Pts',(6.9063217242137,-3.27712490715728,10.622652644332));
#19264=CARTESIAN_POINT('Ctrl Pts',(6.38365961018741,-2.90630232377856,10.70795449752));
#19265=CARTESIAN_POINT('Ctrl Pts',(5.74407957751689,-2.87046702674317,10.7932145497474));
#19266=CARTESIAN_POINT('Ctrl Pts',(5.18413779010185,-3.18009512220889,10.8783879953558));
#19267=CARTESIAN_POINT('Ctrl Pts',(4.87504525063398,-3.73939474085648,10.9634303821887));
#19268=CARTESIAN_POINT('Ctrl Pts',(4.9113280193628,-4.37593360867611,11.0482983399598));
#19269=CARTESIAN_POINT('Ctrl Pts',(5.27937248430205,-4.89450749674953,11.1329488708158));
#19270=CARTESIAN_POINT('Ctrl Pts',(5.86527624347711,-5.13679808752952,11.2173417295453));
#19271=CARTESIAN_POINT('Ctrl Pts',(6.48799534199112,-5.03087191620999,11.3014349903219));
#19272=CARTESIAN_POINT('Ctrl Pts',(6.95693136473707,-4.61090781293032,11.3851957485584));
#19273=CARTESIAN_POINT('Ctrl Pts',(7.07219562678886,-4.21035033769926,11.4407823887657));
#19274=CARTESIAN_POINT('Ctrl Pts',(7.07222266979228,-4.00946826992833,11.4685145081909));
#19275=CARTESIAN_POINT('Origin',(7.,-4.,11.4));
#19276=CARTESIAN_POINT('Origin',(7.,-4.,11.4));
#19277=CARTESIAN_POINT('Origin',(7.,-4.,2.7));
#19278=CARTESIAN_POINT('',(0.,0.,0.));
#19279=CARTESIAN_POINT('Origin',(4.4,6.7,-0.1));
#19280=CARTESIAN_POINT('',(4.19,6.7,0.));
#19281=CARTESIAN_POINT('Origin',(4.4,6.7,0.));
#19282=CARTESIAN_POINT('',(4.19,6.7,0.9));
#19283=CARTESIAN_POINT('',(4.19,6.7,-0.1));
#19284=CARTESIAN_POINT('Origin',(4.4,6.7,0.9));
#19285=CARTESIAN_POINT('Origin',(4.4,6.7,0.9));
#19286=CARTESIAN_POINT('Origin',(7.6,6.7,-0.1));
#19287=CARTESIAN_POINT('',(7.39,6.7,0.));
#19288=CARTESIAN_POINT('Origin',(7.6,6.7,0.));
#19289=CARTESIAN_POINT('',(7.39,6.7,0.9));
#19290=CARTESIAN_POINT('',(7.39,6.7,-0.1));
#19291=CARTESIAN_POINT('Origin',(7.6,6.7,0.9));
#19292=CARTESIAN_POINT('Origin',(7.6,6.7,0.9));
#19293=CARTESIAN_POINT('Origin',(4.4,6.2,1.2));
#19294=CARTESIAN_POINT('',(4.19,6.3,1.2));
#19295=CARTESIAN_POINT('Origin',(4.4,6.3,1.2));
#19296=CARTESIAN_POINT('',(4.19,7.1,1.2));
#19297=CARTESIAN_POINT('',(4.19,6.2,1.2));
#19298=CARTESIAN_POINT('Origin',(4.4,7.1,1.2));
#19299=CARTESIAN_POINT('Origin',(7.6,6.2,1.2));
#19300=CARTESIAN_POINT('',(7.39,6.3,1.2));
#19301=CARTESIAN_POINT('Origin',(7.6,6.3,1.2));
#19302=CARTESIAN_POINT('',(7.39,7.1,1.2));
#19303=CARTESIAN_POINT('',(7.39,6.2,1.2));
#19304=CARTESIAN_POINT('Origin',(7.6,7.1,1.2));
#19305=CARTESIAN_POINT('Origin',(8.4,7.1,0.));
#19306=CARTESIAN_POINT('',(8.4,7.1,0.));
#19307=CARTESIAN_POINT('',(3.6,7.1,0.));
#19308=CARTESIAN_POINT('',(8.4,7.1,0.));
#19309=CARTESIAN_POINT('',(3.6,7.1,3.));
#19310=CARTESIAN_POINT('',(3.6,7.1,0.));
#19311=CARTESIAN_POINT('',(8.4,7.1,3.));
#19312=CARTESIAN_POINT('',(8.4,7.1,3.));
#19313=CARTESIAN_POINT('',(8.4,7.1,0.));
#19314=CARTESIAN_POINT('Origin',(8.4,6.3,0.));
#19315=CARTESIAN_POINT('',(8.4,6.3,0.));
#19316=CARTESIAN_POINT('',(8.4,6.3,0.));
#19317=CARTESIAN_POINT('',(8.4,6.3,3.));
#19318=CARTESIAN_POINT('',(8.4,6.3,3.));
#19319=CARTESIAN_POINT('',(8.4,6.3,0.));
#19320=CARTESIAN_POINT('Origin',(3.6,6.3,0.));
#19321=CARTESIAN_POINT('',(3.6,6.3,0.));
#19322=CARTESIAN_POINT('',(3.6,6.3,0.));
#19323=CARTESIAN_POINT('',(3.6,6.3,3.));
#19324=CARTESIAN_POINT('',(3.6,6.3,3.));
#19325=CARTESIAN_POINT('',(3.6,6.3,0.));
#19326=CARTESIAN_POINT('Origin',(3.6,7.1,0.));
#19327=CARTESIAN_POINT('',(3.6,7.1,0.));
#19328=CARTESIAN_POINT('',(3.6,7.1,3.));
#19329=CARTESIAN_POINT('Origin',(6.,6.7,3.));
#19330=CARTESIAN_POINT('Origin',(6.,6.7,0.));
#19331=CARTESIAN_POINT('',(0.,0.,0.));
#19332=CARTESIAN_POINT('Origin',(4.4,8.,29.6));
#19333=CARTESIAN_POINT('',(4.19,8.,29.7));
#19334=CARTESIAN_POINT('Origin',(4.4,8.,29.7));
#19335=CARTESIAN_POINT('',(4.19,8.,30.5));
#19336=CARTESIAN_POINT('',(4.19,8.,29.6));
#19337=CARTESIAN_POINT('Origin',(4.4,8.,30.5));
#19338=CARTESIAN_POINT('Origin',(7.6,8.,29.6));
#19339=CARTESIAN_POINT('',(7.39,8.,29.7));
#19340=CARTESIAN_POINT('Origin',(7.6,8.,29.7));
#19341=CARTESIAN_POINT('',(7.39,8.,30.5));
#19342=CARTESIAN_POINT('',(7.39,8.,29.6));
#19343=CARTESIAN_POINT('Origin',(7.6,8.,30.5));
#19344=CARTESIAN_POINT('Origin',(4.4,6.2,29.8));
#19345=CARTESIAN_POINT('',(4.19,6.3,29.8));
#19346=CARTESIAN_POINT('Origin',(4.4,6.3,29.8));
#19347=CARTESIAN_POINT('',(4.19,7.2,29.8));
#19348=CARTESIAN_POINT('',(4.19,6.2,29.8));
#19349=CARTESIAN_POINT('',(4.58466185312619,7.2,29.7));
#19350=CARTESIAN_POINT('Origin',(4.4,7.2,29.8));
#19351=CARTESIAN_POINT('',(4.5846618531262,7.1,29.7));
#19352=CARTESIAN_POINT('',(4.58466185312619,6.2,29.7));
#19353=CARTESIAN_POINT('',(4.21533814687381,7.1,29.7));
#19354=CARTESIAN_POINT('Origin',(4.4,7.1,29.8));
#19355=CARTESIAN_POINT('',(4.21533814687381,7.2,29.7));
#19356=CARTESIAN_POINT('',(4.21533814687381,6.2,29.7));
#19357=CARTESIAN_POINT('Origin',(4.4,7.2,29.8));
#19358=CARTESIAN_POINT('Origin',(4.4,7.2,29.8));
#19359=CARTESIAN_POINT('',(6.4,7.2,29.7));
#19360=CARTESIAN_POINT('Origin',(7.6,6.2,29.8));
#19361=CARTESIAN_POINT('',(7.39,6.3,29.8));
#19362=CARTESIAN_POINT('Origin',(7.6,6.3,29.8));
#19363=CARTESIAN_POINT('',(7.39,7.2,29.8));
#19364=CARTESIAN_POINT('',(7.39,6.2,29.8));
#19365=CARTESIAN_POINT('',(7.78466185312619,7.2,29.7));
#19366=CARTESIAN_POINT('Origin',(7.6,7.2,29.8));
#19367=CARTESIAN_POINT('',(7.78466185312619,7.1,29.7));
#19368=CARTESIAN_POINT('',(7.78466185312619,6.2,29.7));
#19369=CARTESIAN_POINT('',(7.4153381468738,7.1,29.7));
#19370=CARTESIAN_POINT('Origin',(7.6,7.1,29.8));
#19371=CARTESIAN_POINT('',(7.41533814687381,7.2,29.7));
#19372=CARTESIAN_POINT('',(7.41533814687381,6.2,29.7));
#19373=CARTESIAN_POINT('Origin',(7.6,7.2,29.8));
#19374=CARTESIAN_POINT('Origin',(7.6,7.2,29.8));
#19375=CARTESIAN_POINT('',(8.,7.2,29.7));
#19376=CARTESIAN_POINT('Origin',(8.4,7.1,28.));
#19377=CARTESIAN_POINT('',(8.4,7.1,29.7));
#19378=CARTESIAN_POINT('',(8.4,7.1,29.7));
#19379=CARTESIAN_POINT('',(8.4,7.1,29.7));
#19380=CARTESIAN_POINT('',(8.4,7.1,28.));
#19381=CARTESIAN_POINT('',(8.4,7.1,28.));
#19382=CARTESIAN_POINT('',(3.6,7.1,28.));
#19383=CARTESIAN_POINT('',(8.4,7.1,28.));
#19384=CARTESIAN_POINT('',(3.6,7.1,29.7));
#19385=CARTESIAN_POINT('',(3.6,7.1,28.));
#19386=CARTESIAN_POINT('',(8.4,7.1,29.7));
#19387=CARTESIAN_POINT('Origin',(8.4,6.3,29.7));
#19388=CARTESIAN_POINT('',(3.6,9.,29.7));
#19389=CARTESIAN_POINT('',(3.6,6.3,29.7));
#19390=CARTESIAN_POINT('',(8.4,9.,29.7));
#19391=CARTESIAN_POINT('',(3.6,9.,29.7));
#19392=CARTESIAN_POINT('',(8.4,6.3,29.7));
#19393=CARTESIAN_POINT('Origin',(6.,9.,30.1));
#19394=CARTESIAN_POINT('',(3.6,9.,30.5));
#19395=CARTESIAN_POINT('',(8.4,9.,30.5));
#19396=CARTESIAN_POINT('',(8.4,9.,30.5));
#19397=CARTESIAN_POINT('',(8.4,9.,29.7));
#19398=CARTESIAN_POINT('',(3.6,9.,30.5));
#19399=CARTESIAN_POINT('Origin',(8.4,6.3,28.));
#19400=CARTESIAN_POINT('',(8.4,6.3,28.));
#19401=CARTESIAN_POINT('',(8.4,6.3,30.5));
#19402=CARTESIAN_POINT('',(8.4,6.3,28.));
#19403=CARTESIAN_POINT('',(8.4,6.3,28.));
#19404=CARTESIAN_POINT('',(8.4,6.3,30.5));
#19405=CARTESIAN_POINT('Origin',(3.6,6.3,28.));
#19406=CARTESIAN_POINT('',(3.6,6.3,28.));
#19407=CARTESIAN_POINT('',(3.6,6.3,30.5));
#19408=CARTESIAN_POINT('',(3.6,6.3,28.));
#19409=CARTESIAN_POINT('',(3.6,6.3,28.));
#19410=CARTESIAN_POINT('',(3.6,6.3,30.5));
#19411=CARTESIAN_POINT('Origin',(3.6,7.1,28.));
#19412=CARTESIAN_POINT('',(3.6,7.1,28.));
#19413=CARTESIAN_POINT('',(3.6,6.3,30.5));
#19414=CARTESIAN_POINT('Origin',(6.,6.7,30.5));
#19415=CARTESIAN_POINT('Origin',(6.,6.7,28.));
#19416=CARTESIAN_POINT('',(0.,0.,0.));
#19417=CARTESIAN_POINT('Origin',(6.,4.,1.9));
#19418=CARTESIAN_POINT('',(5.375,4.,2.6));
#19419=CARTESIAN_POINT('Origin',(6.,4.,2.6));
#19420=CARTESIAN_POINT('',(5.375,4.,1.9));
#19421=CARTESIAN_POINT('',(5.375,4.,1.9));
#19422=CARTESIAN_POINT('Origin',(6.,4.,1.9));
#19423=CARTESIAN_POINT('Origin',(6.,4.,1.9));
#19424=CARTESIAN_POINT('',(4.5,4.,2.6));
#19425=CARTESIAN_POINT('Origin',(6.,4.,2.6));
#19426=CARTESIAN_POINT('',(4.5,4.,1.9));
#19427=CARTESIAN_POINT('',(4.5,4.,1.9));
#19428=CARTESIAN_POINT('Origin',(6.,4.,1.9));
#19429=CARTESIAN_POINT('Origin',(6.,4.,2.6));
#19430=CARTESIAN_POINT('Origin',(6.,4.,1.9));
#19431=CARTESIAN_POINT('',(0.,0.,0.));
#19432=CARTESIAN_POINT('Ctrl Pts',(6.99999815899373,4.01367547347479,2.60093950625072));
#19433=CARTESIAN_POINT('Ctrl Pts',(6.99997288064589,4.20144961727953,2.62686205390015));
#19434=CARTESIAN_POINT('Ctrl Pts',(6.89230845853935,4.57620131355266,2.67882572810781));
#19435=CARTESIAN_POINT('Ctrl Pts',(6.45268902055693,4.97011892113672,2.75738771144581));
#19436=CARTESIAN_POINT('Ctrl Pts',(5.86669155617951,5.07009441973235,2.83651805910941));
#19437=CARTESIAN_POINT('Ctrl Pts',(5.31323924231124,4.84148977638369,2.91622570222972));
#19438=CARTESIAN_POINT('Ctrl Pts',(4.96382442320151,4.34995448969575,2.99649058141579));
#19439=CARTESIAN_POINT('Ctrl Pts',(4.92922815468166,3.74381008719936,3.07730076310524));
#19440=CARTESIAN_POINT('Ctrl Pts',(5.22433988671615,3.20870475874992,3.15863604084508));
#19441=CARTESIAN_POINT('Ctrl Pts',(5.76222017520179,2.91082295270622,3.24047540691231));
#19442=CARTESIAN_POINT('Ctrl Pts',(6.37972244802771,2.94499376197989,3.3227938596108));
#19443=CARTESIAN_POINT('Ctrl Pts',(6.88714214280083,3.30444617999842,3.40556405334158));
#19444=CARTESIAN_POINT('Ctrl Pts',(7.1267179261553,3.88170395597293,3.48875576611263));
#19445=CARTESIAN_POINT('Ctrl Pts',(7.02193956541344,4.50081591971197,3.57233637082151));
#19446=CARTESIAN_POINT('Ctrl Pts',(6.60200309921583,4.97124649007052,3.65627092163634));
#19447=CARTESIAN_POINT('Ctrl Pts',(5.99391816782283,5.1467637293928,3.74052239101179));
#19448=CARTESIAN_POINT('Ctrl Pts',(5.38351410020794,4.97125258500565,3.82505187835831));
#19449=CARTESIAN_POINT('Ctrl Pts',(4.97495278641361,4.51407471129711,3.90667930564871));
#19450=CARTESIAN_POINT('Ctrl Pts',(4.85890493436876,3.9395318134167,3.98533819655606));
#19451=CARTESIAN_POINT('Ctrl Pts',(5.0248445336464,3.40104453051283,4.06097495851984));
#19452=CARTESIAN_POINT('Ctrl Pts',(5.42877344681216,3.00706135834947,4.13670514776413));
#19453=CARTESIAN_POINT('Ctrl Pts',(5.97224138292893,2.85377277882407,4.21249751166765));
#19454=CARTESIAN_POINT('Ctrl Pts',(6.52306794486814,2.97976887786423,4.28832050304671));
#19455=CARTESIAN_POINT('Ctrl Pts',(6.911106619782,3.32248792481664,4.35782394345616));
#19456=CARTESIAN_POINT('Ctrl Pts',(7.09651656274147,3.74815778477591,4.4209850314008));
#19457=CARTESIAN_POINT('Ctrl Pts',(7.11222142726568,4.16541427135673,4.47779829351342));
#19458=CARTESIAN_POINT('Ctrl Pts',(6.97427650626816,4.55914085431083,4.53456660987697));
#19459=CARTESIAN_POINT('Ctrl Pts',(6.6723790417336,4.91046294860728,4.59757802409045));
#19460=CARTESIAN_POINT('Ctrl Pts',(6.20229995228089,5.12240612151564,4.66678931423933));
#19461=CARTESIAN_POINT('Ctrl Pts',(5.6425500433818,5.08009523000915,4.74213609069821));
#19462=CARTESIAN_POINT('Ctrl Pts',(5.21136094690014,4.8013569526932,4.8110335703418));
#19463=CARTESIAN_POINT('Ctrl Pts',(4.96782069609662,4.41239190726546,4.87351124705845));
#19464=CARTESIAN_POINT('Ctrl Pts',(4.86407127402864,3.87207825314686,4.94830807657783));
#19465=CARTESIAN_POINT('Ctrl Pts',(5.12715288076494,3.20107434287668,5.041444793684));
#19466=CARTESIAN_POINT('Ctrl Pts',(5.90376531288412,2.82823955973182,5.15254762811187));
#19467=CARTESIAN_POINT('Ctrl Pts',(6.72029013273465,3.08146453910134,5.2629101070658));
#19468=CARTESIAN_POINT('Ctrl Pts',(7.14364665428008,3.81715099008766,5.37246078991918));
#19469=CARTESIAN_POINT('Ctrl Pts',(6.9551205530812,4.63769652624648,5.4811367937548));
#19470=CARTESIAN_POINT('Ctrl Pts',(6.2641024490546,5.1069317667711,5.5888844628491));
#19471=CARTESIAN_POINT('Ctrl Pts',(5.62881174521816,5.00949357808685,5.67193196549233));
#19472=CARTESIAN_POINT('Ctrl Pts',(5.2874560242671,4.74926815537235,5.73087908447157));
#19473=CARTESIAN_POINT('Ctrl Pts',(5.07381541095866,4.48213637560843,5.77788659685938));
#19474=CARTESIAN_POINT('Ctrl Pts',(4.94552168624609,4.06557538718633,5.83636209008294));
#19475=CARTESIAN_POINT('Ctrl Pts',(5.04911869155687,3.55670415977292,5.90607316299982));
#19476=CARTESIAN_POINT('Ctrl Pts',(5.38099173791495,3.16160536520236,5.97532164753646));
#19477=CARTESIAN_POINT('Ctrl Pts',(5.85816561666817,2.97493727370523,6.04410657341625));
#19478=CARTESIAN_POINT('Ctrl Pts',(6.32119024886796,3.03347138881056,6.1067356435835));
#19479=CARTESIAN_POINT('Ctrl Pts',(6.67264815667528,3.25520245847479,6.16333652453463));
#19480=CARTESIAN_POINT('Ctrl Pts',(6.9689172446974,3.65479400388877,6.23091649769543));
#19481=CARTESIAN_POINT('Ctrl Pts',(7.0079089842411,4.17131843581214,6.29799027327548));
#19482=CARTESIAN_POINT('Ctrl Pts',(6.77691391923214,4.60388596675421,6.36457330679182));
#19483=CARTESIAN_POINT('Ctrl Pts',(6.50054973430609,4.84205531318333,6.414270318429));
#19484=CARTESIAN_POINT('Ctrl Pts',(6.15708960805529,4.96183696463414,6.46373244636263));
#19485=CARTESIAN_POINT('Ctrl Pts',(5.73515865256543,4.94625066250657,6.52117144063107));
#19486=CARTESIAN_POINT('Ctrl Pts',(5.30609465295405,4.70907742816445,6.5864458994691));
#19487=CARTESIAN_POINT('Ctrl Pts',(5.04126574291307,4.22881801076535,6.65940509117474));
#19488=CARTESIAN_POINT('Ctrl Pts',(5.06730780646012,3.7758858483265,6.71983222415362));
#19489=CARTESIAN_POINT('Ctrl Pts',(5.22892555890349,3.46412922360998,6.7679659145206));
#19490=CARTESIAN_POINT('Ctrl Pts',(5.4292015128227,3.25210405867328,6.80796630929891));
#19491=CARTESIAN_POINT('Ctrl Pts',(5.71433691472614,3.10148200562693,6.85183024183257));
#19492=CARTESIAN_POINT('Ctrl Pts',(6.06256514105404,3.06238687711817,6.89952195897341));
#19493=CARTESIAN_POINT('Ctrl Pts',(6.4564976195634,3.16770820022483,6.95498839068538));
#19494=CARTESIAN_POINT('Ctrl Pts',(6.8102288164166,3.48372159458398,7.01814871427154));
#19495=CARTESIAN_POINT('Ctrl Pts',(6.95714247630162,3.9949743218129,7.08893288176131));
#19496=CARTESIAN_POINT('Ctrl Pts',(6.81021696910949,4.50416338125004,7.1594866624322));
#19497=CARTESIAN_POINT('Ctrl Pts',(6.41591912974157,4.85632155826513,7.22985222666365));
#19498=CARTESIAN_POINT('Ctrl Pts',(5.89581150258709,4.9445435848153,7.30007283488175));
#19499=CARTESIAN_POINT('Ctrl Pts',(5.4091541149686,4.74288106481787,7.37019262264602));
#19500=CARTESIAN_POINT('Ctrl Pts',(5.1045916955003,4.31357351873737,7.4402563254929));
#19501=CARTESIAN_POINT('Ctrl Pts',(5.07507074796588,3.78812027671986,7.51030900575102));
#19502=CARTESIAN_POINT('Ctrl Pts',(5.32971571962661,3.32725097083008,7.58039577698861));
#19503=CARTESIAN_POINT('Ctrl Pts',(5.79102376728976,3.07217291555275,7.65056157443439));
#19504=CARTESIAN_POINT('Ctrl Pts',(6.31826217852957,3.10162768020774,7.72085085716367));
#19505=CARTESIAN_POINT('Ctrl Pts',(6.75007083293795,3.40776502742426,7.79130734598018));
#19506=CARTESIAN_POINT('Ctrl Pts',(6.95345754831281,3.89815513784294,7.86197377424134));
#19507=CARTESIAN_POINT('Ctrl Pts',(6.86450758322969,4.42345798565047,7.9328916442996));
#19508=CARTESIAN_POINT('Ctrl Pts',(6.50825373195115,4.82258144361629,8.00410096577401));
#19509=CARTESIAN_POINT('Ctrl Pts',(5.99196133471143,4.97171282731416,8.07564000535001));
#19510=CARTESIAN_POINT('Ctrl Pts',(5.47264846544098,4.82257977354425,8.14754510597589));
#19511=CARTESIAN_POINT('Ctrl Pts',(5.12402089676511,4.43277938176583,8.21717246163365));
#19512=CARTESIAN_POINT('Ctrl Pts',(5.02434526751946,3.94102818280025,8.28449961898673));
#19513=CARTESIAN_POINT('Ctrl Pts',(5.16694197219437,3.47827882962972,8.34949563910625));
#19514=CARTESIAN_POINT('Ctrl Pts',(5.48619587513468,3.16623898773365,8.40942447363167));
#19515=CARTESIAN_POINT('Ctrl Pts',(5.86631955340104,3.03340212556353,8.46419547601151));
#19516=CARTESIAN_POINT('Ctrl Pts',(6.22999033724363,3.04672408117636,8.5137197912885));
#19517=CARTESIAN_POINT('Ctrl Pts',(6.56525962631825,3.19292643023923,8.5634804916257));
#19518=CARTESIAN_POINT('Ctrl Pts',(6.82522778577244,3.45264122124887,8.61348288970028));
#19519=CARTESIAN_POINT('Ctrl Pts',(6.97307814435936,3.7910761621246,8.66373168303779));
#19520=CARTESIAN_POINT('Ctrl Pts',(6.98712736643486,4.16195247500926,8.71423091450252));
#19521=CARTESIAN_POINT('Ctrl Pts',(6.86409623902891,4.5140922960367,8.76498396821101));
#19522=CARTESIAN_POINT('Ctrl Pts',(6.61968565405262,4.79836651831856,8.81599356006379));
#19523=CARTESIAN_POINT('Ctrl Pts',(6.28663324217223,4.97458782653242,8.86726173278701));
#19524=CARTESIAN_POINT('Ctrl Pts',(5.9103163648716,5.01715912899264,8.91878984727219));
#19525=CARTESIAN_POINT('Ctrl Pts',(5.5426151162157,4.91881558382611,8.97057858184767));
#19526=CARTESIAN_POINT('Ctrl Pts',(5.2346932137367,4.69177671709244,9.02262792714338));
#19527=CARTESIAN_POINT('Ctrl Pts',(5.03002927873253,4.36635777160092,9.07493719269484));
#19528=CARTESIAN_POINT('Ctrl Pts',(4.95793528493379,3.98670141138964,9.12750499446544));
#19529=CARTESIAN_POINT('Ctrl Pts',(5.03011221582078,3.60530312678215,9.18032928985668));
#19530=CARTESIAN_POINT('Ctrl Pts',(5.26028491013977,3.23792219176526,9.23930487837506));
#19531=CARTESIAN_POINT('Ctrl Pts',(5.66833767471456,2.97390330572424,9.30453505298122));
#19532=CARTESIAN_POINT('Ctrl Pts',(6.20020835504347,2.93396150339657,9.37613052320119));
#19533=CARTESIAN_POINT('Ctrl Pts',(6.70998344550478,3.16323515745987,9.45115011118038));
#19534=CARTESIAN_POINT('Ctrl Pts',(7.05174463296735,3.64363058779886,9.52964181253653));
#19535=CARTESIAN_POINT('Ctrl Pts',(7.08674491429888,4.25878461683797,9.61164803498578));
#19536=CARTESIAN_POINT('Ctrl Pts',(6.78746221281555,4.80126791369132,9.69412424256602));
#19537=CARTESIAN_POINT('Ctrl Pts',(6.24245359179364,5.10299460367291,9.77704205650278));
#19538=CARTESIAN_POINT('Ctrl Pts',(5.617389337803,5.06829072683056,9.86037045574097));
#19539=CARTESIAN_POINT('Ctrl Pts',(5.10428990247565,4.70469241242162,9.94407602255943));
#19540=CARTESIAN_POINT('Ctrl Pts',(4.86233610468105,4.12145238678417,10.0281230884956));
#19541=CARTESIAN_POINT('Ctrl Pts',(4.96818752346366,3.49664100367693,10.1124739581892));
#19542=CARTESIAN_POINT('Ctrl Pts',(5.39158733307429,3.02246211865203,10.197089152739));
#19543=CARTESIAN_POINT('Ctrl Pts',(6.00398991824946,2.84580444666258,10.2819276236503));
#19544=CARTESIAN_POINT('Ctrl Pts',(6.61780477214459,3.0224619351938,10.3669470022194));
#19545=CARTESIAN_POINT('Ctrl Pts',(7.04420003577297,3.49941215707345,10.4521038303345));
#19546=CARTESIAN_POINT('Ctrl Pts',(7.15155414725,4.13081128487796,10.5373538665558));
#19547=CARTESIAN_POINT('Ctrl Pts',(6.90634183228622,4.72286458915024,10.6226522963591));
#19548=CARTESIAN_POINT('Ctrl Pts',(6.38367034420738,5.09368398946472,10.7079540131199));
#19549=CARTESIAN_POINT('Ctrl Pts',(5.74412845724406,5.12951897848491,10.7932138931513));
#19550=CARTESIAN_POINT('Ctrl Pts',(5.18413119725411,4.81987766303419,10.8783870658711));
#19551=CARTESIAN_POINT('Ctrl Pts',(4.8752129919825,4.26058851376116,10.9634291554075));
#19552=CARTESIAN_POINT('Ctrl Pts',(4.91115871222138,3.62399076997319,11.0482965295163));
#19553=CARTESIAN_POINT('Ctrl Pts',(5.27935908785992,3.10540850794678,11.1329466617017));
#19554=CARTESIAN_POINT('Ctrl Pts',(5.86521072908837,2.86304864268273,11.2173381122335));
#19555=CARTESIAN_POINT('Ctrl Pts',(6.48796989668153,2.969020134583,11.3014313415043));
#19556=CARTESIAN_POINT('Ctrl Pts',(6.95689206969945,3.38875839075872,11.3851878190745));
#19557=CARTESIAN_POINT('Ctrl Pts',(7.07219562678887,3.7896496622666,11.4407823887692));
#19558=CARTESIAN_POINT('Ctrl Pts',(7.07222266979222,3.99053173007441,11.4685145081913));
#19559=CARTESIAN_POINT('Ctrl Pts',(6.97007822923066,4.01367144562316,2.60093950625072));
#19560=CARTESIAN_POINT('Ctrl Pts',(6.97005368434554,4.19599723746873,2.62610989942131));
#19561=CARTESIAN_POINT('Ctrl Pts',(6.86557136883425,4.55976104448084,2.67654110363146));
#19562=CARTESIAN_POINT('Ctrl Pts',(6.43865008190508,4.94238932286108,2.75283713480025));
#19563=CARTESIAN_POINT('Ctrl Pts',(5.86921493316712,5.03959284630734,2.82972340130287));
#19564=CARTESIAN_POINT('Ctrl Pts',(5.33096558193683,4.81735099663587,2.90723060147415));
#19565=CARTESIAN_POINT('Ctrl Pts',(4.99079371715267,4.33896249921493,2.98534758100617));
#19566=CARTESIAN_POINT('Ctrl Pts',(4.95698752448753,3.74836627630877,3.06407671089558));
#19567=CARTESIAN_POINT('Ctrl Pts',(5.2447735927993,3.2263183390518,3.14340920265259));
#19568=CARTESIAN_POINT('Ctrl Pts',(5.77009659483826,2.935253839257,3.22333615530246));
#19569=CARTESIAN_POINT('Ctrl Pts',(6.37410700305503,2.96854764545913,3.3038436660997));
#19570=CARTESIAN_POINT('Ctrl Pts',(6.87126720532805,3.32056148618083,3.38491508906228));
#19571=CARTESIAN_POINT('Ctrl Pts',(7.10647606519176,3.8869115704884,3.46653020083125));
#19572=CARTESIAN_POINT('Ctrl Pts',(7.00364598168452,4.49544455922231,3.54866556866602));
#19573=CARTESIAN_POINT('Ctrl Pts',(6.59029031467595,4.95874770146656,3.63129490508721));
#19574=CARTESIAN_POINT('Ctrl Pts',(5.99050118891129,5.13204649144633,3.71438838994562));
#19575=CARTESIAN_POINT('Ctrl Pts',(5.3871831217877,4.95875602570457,3.7979148029937));
#19576=CARTESIAN_POINT('Ctrl Pts',(4.98248033378271,4.5061541351041,3.87872893188492));
#19577=CARTESIAN_POINT('Ctrl Pts',(4.86721670822546,3.93617018411993,3.9567542866616));
#19578=CARTESIAN_POINT('Ctrl Pts',(5.03201656034403,3.40093722969711,4.03191362348647));
#19579=CARTESIAN_POINT('Ctrl Pts',(5.4341155083194,3.00856657873451,4.10730454881205));
#19580=CARTESIAN_POINT('Ctrl Pts',(5.97619334481198,2.85552532694299,4.18289846038133));
#19581=CARTESIAN_POINT('Ctrl Pts',(6.52668855342533,2.98131870321029,4.25866237838478));
#19582=CARTESIAN_POINT('Ctrl Pts',(6.91525015578364,3.32433290152934,4.32823137789653));
#19583=CARTESIAN_POINT('Ctrl Pts',(7.10122540761753,3.75115514096909,4.39155786672224));
#19584=CARTESIAN_POINT('Ctrl Pts',(7.11704685769188,4.17012217382455,4.44859651091126));
#19585=CARTESIAN_POINT('Ctrl Pts',(6.97839397277603,4.56601865778953,4.50566782536761));
#19586=CARTESIAN_POINT('Ctrl Pts',(6.67448841900728,4.91976294635959,4.56909884830092));
#19587=CARTESIAN_POINT('Ctrl Pts',(6.20052248645988,5.13357708557862,4.63887978848427));
#19588=CARTESIAN_POINT('Ctrl Pts',(5.63509567281091,5.09095185636156,4.71498366372174));
#19589=CARTESIAN_POINT('Ctrl Pts',(5.19876269746781,4.80900916922666,4.78468292309207));
#19590=CARTESIAN_POINT('Ctrl Pts',(4.95194713053102,4.41489646436617,4.84798451555781));
#19591=CARTESIAN_POINT('Ctrl Pts',(4.84663163915403,3.86676853344418,4.92386073086651));
#19592=CARTESIAN_POINT('Ctrl Pts',(5.11372101102488,3.18474837462606,5.0184947367369));
#19593=CARTESIAN_POINT('Ctrl Pts',(5.90458358669118,2.80468201966577,5.13164482139767));
#19594=CARTESIAN_POINT('Ctrl Pts',(6.73806869810391,3.06284081116781,5.24427216882798));
#19595=CARTESIAN_POINT('Ctrl Pts',(7.17122830583924,3.81499585651111,5.35628592540322));
#19596=CARTESIAN_POINT('Ctrl Pts',(6.97836567750197,4.65554163951089,5.4675943780275));
#19597=CARTESIAN_POINT('Ctrl Pts',(6.26962123406518,5.13706960433728,5.57811808279645));
#19598=CARTESIAN_POINT('Ctrl Pts',(5.6171015280907,5.03711333283845,5.66341094659106));
#19599=CARTESIAN_POINT('Ctrl Pts',(5.26625724402755,4.76966136409525,5.72399491793109));
#19600=CARTESIAN_POINT('Ctrl Pts',(5.0466141008817,4.49503234360151,5.77232232410499));
#19601=CARTESIAN_POINT('Ctrl Pts',(4.91464587553303,4.06660447798485,5.83246573595406));
#19602=CARTESIAN_POINT('Ctrl Pts',(5.02121955424947,3.54300221950532,5.90419392967494));
#19603=CARTESIAN_POINT('Ctrl Pts',(5.36279729464331,3.13634388271878,5.97547169397601));
#19604=CARTESIAN_POINT('Ctrl Pts',(5.85400629104318,2.94418099963678,6.04628110835755));
#19605=CARTESIAN_POINT('Ctrl Pts',(6.33067382166986,3.00445097853177,6.11075992168625));
#19606=CARTESIAN_POINT('Ctrl Pts',(6.69244602053762,3.23270120290387,6.1690265414894));
#19607=CARTESIAN_POINT('Ctrl Pts',(6.99736200274051,3.64397358611959,6.23858290813363));
#19608=CARTESIAN_POINT('Ctrl Pts',(7.03741327745268,4.17541560408681,6.30760225841541));
#19609=CARTESIAN_POINT('Ctrl Pts',(6.79986566660976,4.6201895916107,6.37607276037605));
#19610=CARTESIAN_POINT('Ctrl Pts',(6.51581397770933,4.86495817257182,6.42715430300098));
#19611=CARTESIAN_POINT('Ctrl Pts',(6.16299958122418,4.9879746007512,6.47796790685504));
#19612=CARTESIAN_POINT('Ctrl Pts',(5.7298601965859,4.97194208493422,6.53693785301752));
#19613=CARTESIAN_POINT('Ctrl Pts',(5.28981334339032,4.7285935869624,6.60390272317146));
#19614=CARTESIAN_POINT('Ctrl Pts',(5.01861530795073,4.23654965453147,6.67865419687793));
#19615=CARTESIAN_POINT('Ctrl Pts',(5.04535351427297,3.77319789368563,6.740486484592));
#19616=CARTESIAN_POINT('Ctrl Pts',(5.21050707940139,3.45466912378663,6.78967190151324));
#19617=CARTESIAN_POINT('Ctrl Pts',(5.41498846216358,3.23821604795383,6.83051376083048));
#19618=CARTESIAN_POINT('Ctrl Pts',(5.70582623070768,3.08462360380577,6.87525912610462));
#19619=CARTESIAN_POINT('Ctrl Pts',(6.06055931995987,3.04484118040771,6.92384480353423));
#19620=CARTESIAN_POINT('Ctrl Pts',(6.4613286018102,3.1520453317179,6.98028088520478));
#19621=CARTESIAN_POINT('Ctrl Pts',(6.82054281279478,3.47314701577422,7.044453443696));
#19622=CARTESIAN_POINT('Ctrl Pts',(6.96928903457135,3.99139090417698,7.11621304917794));
#19623=CARTESIAN_POINT('Ctrl Pts',(6.82053867569686,4.50630577580192,7.18758304630547));
#19624=CARTESIAN_POINT('Ctrl Pts',(6.4225779203956,4.86150106821318,7.2585967677241));
#19625=CARTESIAN_POINT('Ctrl Pts',(5.89901648989417,4.95012788622332,7.32929565353266));
#19626=CARTESIAN_POINT('Ctrl Pts',(5.41042086398466,4.74746463183478,7.39972027350523));
#19627=CARTESIAN_POINT('Ctrl Pts',(5.10551074979547,4.31734756146974,7.46991401153098));
#19628=CARTESIAN_POINT('Ctrl Pts',(5.07619993383651,3.7923384190453,7.53992105125218));
#19629=CARTESIAN_POINT('Ctrl Pts',(5.33014973735899,3.33310630778287,7.60978689821025));
#19630=CARTESIAN_POINT('Ctrl Pts',(5.78885557715137,3.07967280968343,7.67955779837817));
#19631=CARTESIAN_POINT('Ctrl Pts',(6.31173203548677,3.10905948858246,7.74928060123239));
#19632=CARTESIAN_POINT('Ctrl Pts',(6.73885834106689,3.4120851493114,7.81900239890985));
#19633=CARTESIAN_POINT('Ctrl Pts',(6.93947166032782,3.89621327586067,7.88877032957341));
#19634=CARTESIAN_POINT('Ctrl Pts',(6.8517095108915,4.41356978513471,7.95863121731408));
#19635=CARTESIAN_POINT('Ctrl Pts',(6.5014540891724,4.80575205348109,8.02863146926931));
#19636=CARTESIAN_POINT('Ctrl Pts',(5.99497523815052,4.95190598589647,8.09881638421139));
#19637=CARTESIAN_POINT('Ctrl Pts',(5.48654071069358,4.80576306205798,8.16923084285141));
#19638=CARTESIAN_POINT('Ctrl Pts',(5.14584576047594,4.42467139458698,8.23729904032951));
#19639=CARTESIAN_POINT('Ctrl Pts',(5.04862865635048,3.94466948422526,8.30302425242081));
#19640=CARTESIAN_POINT('Ctrl Pts',(5.1876995521521,3.4935673709884,8.36639115082881));
#19641=CARTESIAN_POINT('Ctrl Pts',(5.49863720452088,3.18973076893938,8.42475458722929));
#19642=CARTESIAN_POINT('Ctrl Pts',(5.86851760288087,3.0604931366299,8.4780527344378));
#19643=CARTESIAN_POINT('Ctrl Pts',(6.22216787595036,3.07346286057778,8.52621481691567));
#19644=CARTESIAN_POINT('Ctrl Pts',(6.5480141776102,3.21557057599501,8.57457904463358));
#19645=CARTESIAN_POINT('Ctrl Pts',(6.80056307052306,3.4678858151066,8.62315683051673));
#19646=CARTESIAN_POINT('Ctrl Pts',(6.94413931041581,3.79655103609974,8.67195575349977));
#19647=CARTESIAN_POINT('Ctrl Pts',(6.95777663896381,4.1566166576575,8.72098348001793));
#19648=CARTESIAN_POINT('Ctrl Pts',(6.83835640468416,4.49842325083042,8.77024736714704));
#19649=CARTESIAN_POINT('Ctrl Pts',(6.60114870934877,4.77432525687952,8.81975397758997));
#19650=CARTESIAN_POINT('Ctrl Pts',(6.27792266149878,4.94535449549104,8.86950937083879));
#19651=CARTESIAN_POINT('Ctrl Pts',(5.91269004632584,4.9866810736209,8.91951878295217));
#19652=CARTESIAN_POINT('Ctrl Pts',(5.55577147754238,4.89123310443155,8.96978710902608));
#19653=CARTESIAN_POINT('Ctrl Pts',(5.25681276570615,4.67082116051935,9.02031786464434));
#19654=CARTESIAN_POINT('Ctrl Pts',(5.05804412704128,4.35480348104479,9.07111543725805));
#19655=CARTESIAN_POINT('Ctrl Pts',(4.98798705777152,3.98598291367431,9.12218002825493));
#19656=CARTESIAN_POINT('Ctrl Pts',(5.05811977792938,3.61529667809049,9.17351899333755));
#19657=CARTESIAN_POINT('Ctrl Pts',(5.28190831721568,3.25805572249925,9.23086036879321));
#19658=CARTESIAN_POINT('Ctrl Pts',(5.67891985984916,3.00111868286535,9.29432522451153));
#19659=CARTESIAN_POINT('Ctrl Pts',(6.19688560491034,2.9621595442335,9.36404551126668));
#19660=CARTESIAN_POINT('Ctrl Pts',(6.69384264119656,3.1855841651649,9.43716571018052));
#19661=CARTESIAN_POINT('Ctrl Pts',(7.02745653769267,3.65434324756386,9.51375564449963));
#19662=CARTESIAN_POINT('Ctrl Pts',(7.06178183126963,4.2554746146398,9.5938821811463));
#19663=CARTESIAN_POINT('Ctrl Pts',(6.76900853890664,4.78642987830011,9.67458399011126));
#19664=CARTESIAN_POINT('Ctrl Pts',(6.2348861539486,5.08229107067811,9.75584346418169));
#19665=CARTESIAN_POINT('Ctrl Pts',(5.62121277322736,5.04836986639924,9.83763914147065));
#19666=CARTESIAN_POINT('Ctrl Pts',(5.11650932635337,4.69091474437354,9.91994668477699));
#19667=CARTESIAN_POINT('Ctrl Pts',(4.87797688353407,4.11635214273989,10.0027386196848));
#19668=CARTESIAN_POINT('Ctrl Pts',(4.98229143524868,3.49959194392981,10.0859846604355));
#19669=CARTESIAN_POINT('Ctrl Pts',(5.40088841551943,3.03052905348384,10.1696518328908));
#19670=CARTESIAN_POINT('Ctrl Pts',(6.00767495654909,2.85530554851361,10.2537046813517));
#19671=CARTESIAN_POINT('Ctrl Pts',(6.61717928387298,3.0305340090082,10.3381054688078));
#19672=CARTESIAN_POINT('Ctrl Pts',(7.04154155207535,3.50493616550168,10.4228143856807));
#19673=CARTESIAN_POINT('Ctrl Pts',(7.14874926349887,4.13438019996447,10.5077898264163));
#19674=CARTESIAN_POINT('Ctrl Pts',(6.903950445343,4.72591482840965,10.5929885893347));
#19675=CARTESIAN_POINT('Ctrl Pts',(6.38082968565313,5.097277921466,10.6783661408612));
#19676=CARTESIAN_POINT('Ctrl Pts',(5.73930584472151,5.1334076879623,10.7638768930001));
#19677=CARTESIAN_POINT('Ctrl Pts',(5.1763348259103,4.82233123796325,10.8494744602056));
#19678=CARTESIAN_POINT('Ctrl Pts',(4.86504358341962,4.25912384558844,10.9351119396295));
#19679=CARTESIAN_POINT('Ctrl Pts',(4.90113867988794,3.616695945718,11.0207420968181));
#19680=CARTESIAN_POINT('Ctrl Pts',(5.27327395706588,3.09227155786067,11.1063179162021));
#19681=CARTESIAN_POINT('Ctrl Pts',(5.86665748296697,2.84661645816999,11.191792220633));
#19682=CARTESIAN_POINT('Ctrl Pts',(6.49864602437145,2.95402097485745,11.2771193627449));
#19683=CARTESIAN_POINT('Ctrl Pts',(6.97542925162609,3.38059696423684,11.3622524435191));
#19684=CARTESIAN_POINT('Ctrl Pts',(7.09288943197316,3.78884348331495,11.4188571787932));
#19685=CARTESIAN_POINT('Ctrl Pts',(7.09291698096067,3.9934841256345,11.4471081759746));
#19686=CARTESIAN_POINT('Ctrl Pts',(6.91041395631137,4.00974220039509,2.62934344456));
#19687=CARTESIAN_POINT('Ctrl Pts',(6.91039088332254,4.18113436374074,2.65300443127011));
#19688=CARTESIAN_POINT('Ctrl Pts',(6.81223276212051,4.52255345520787,2.70034331641334));
#19689=CARTESIAN_POINT('Ctrl Pts',(6.41194642259563,4.88120070727789,2.77187314650894));
#19690=CARTESIAN_POINT('Ctrl Pts',(5.87867709505731,4.97214216865051,2.84387604072737));
#19691=CARTESIAN_POINT('Ctrl Pts',(5.37495924775045,4.76411517635802,2.91641695294443));
#19692=CARTESIAN_POINT('Ctrl Pts',(5.05668129740466,4.31649040506209,2.98951203519711));
#19693=CARTESIAN_POINT('Ctrl Pts',(5.02502510535536,3.76378693926526,3.06319455885174));
#19694=CARTESIAN_POINT('Ctrl Pts',(5.29445839813617,3.27492491430021,3.13748525737848));
#19695=CARTESIAN_POINT('Ctrl Pts',(5.7867927450234,3.00204415093235,3.21240536311296));
#19696=CARTESIAN_POINT('Ctrl Pts',(6.35367476207417,3.03317811376964,3.28797059030528));
#19697=CARTESIAN_POINT('Ctrl Pts',(6.82113294013823,3.36398710098779,3.3641936508289));
#19698=CARTESIAN_POINT('Ctrl Pts',(7.04285181628566,3.89741148229682,3.44108302054775));
#19699=CARTESIAN_POINT('Ctrl Pts',(6.94595725577566,4.47200025222025,3.51864340064914));
#19700=CARTESIAN_POINT('Ctrl Pts',(6.55482461724248,4.91072870029518,3.59687544889804));
#19701=CARTESIAN_POINT('Ctrl Pts',(5.98546700894343,5.07548895052134,3.6757759027718));
#19702=CARTESIAN_POINT('Ctrl Pts',(5.410813879295,4.91071249002105,3.75533749097694));
#19703=CARTESIAN_POINT('Ctrl Pts',(5.02387704038526,4.47839131136037,3.83257833326237));
#19704=CARTESIAN_POINT('Ctrl Pts',(4.91313809632786,3.93191629171446,3.90740358805855));
#19705=CARTESIAN_POINT('Ctrl Pts',(5.07147125606051,3.41693922450177,3.97972471031443));
#19706=CARTESIAN_POINT('Ctrl Pts',(5.45948459805726,3.03797547396936,4.05251873428609));
#19707=CARTESIAN_POINT('Ctrl Pts',(5.98460263169843,2.889479086358,4.12576876881835));
#19708=CARTESIAN_POINT('Ctrl Pts',(6.51998892431244,3.01154612450741,4.19945421987059));
#19709=CARTESIAN_POINT('Ctrl Pts',(6.89944541092262,3.34622177075522,4.26738065081938));
#19710=CARTESIAN_POINT('Ctrl Pts',(7.08171822960832,3.76422693672321,4.32941579049949));
#19711=CARTESIAN_POINT('Ctrl Pts',(7.09737243151346,4.17579142315723,4.38545681087643));
#19712=CARTESIAN_POINT('Ctrl Pts',(6.96087151461153,4.5658912546307,4.44169554493835));
#19713=CARTESIAN_POINT('Ctrl Pts',(6.66065391126806,4.91555058236023,4.50439030579462));
#19714=CARTESIAN_POINT('Ctrl Pts',(6.1907350383217,5.12782606208152,4.57360248255073));
#19715=CARTESIAN_POINT('Ctrl Pts',(5.6277311318136,5.08567703703038,4.64938413671657));
#19716=CARTESIAN_POINT('Ctrl Pts',(5.19135680604461,4.80403271882307,4.71908080648419));
#19717=CARTESIAN_POINT('Ctrl Pts',(4.94362412438308,4.40869780521622,4.78259619492735));
#19718=CARTESIAN_POINT('Ctrl Pts',(4.83748052823326,3.85720781418724,4.85895645195229));
#19719=CARTESIAN_POINT('Ctrl Pts',(5.10669909946152,3.16750117053444,4.95464506809566));
#19720=CARTESIAN_POINT('Ctrl Pts',(5.91041143557091,2.78013675935754,5.06971853993261));
#19721=CARTESIAN_POINT('Ctrl Pts',(6.76309387143705,3.04322489315909,5.18492407896373));
#19722=CARTESIAN_POINT('Ctrl Pts',(7.20935006792413,3.81626935637355,5.30013664261463));
#19723=CARTESIAN_POINT('Ctrl Pts',(7.0108130147558,4.68549349365627,5.41523674764503));
#19724=CARTESIAN_POINT('Ctrl Pts',(6.27479660211849,5.18656709146719,5.53009928355427));
#19725=CARTESIAN_POINT('Ctrl Pts',(5.59341579180994,5.08278127978539,5.61916691846602));
#19726=CARTESIAN_POINT('Ctrl Pts',(5.22600755552765,4.80276063146936,5.68260544526989));
#19727=CARTESIAN_POINT('Ctrl Pts',(4.99568102716636,4.51482585519067,5.73328066698038));
#19728=CARTESIAN_POINT('Ctrl Pts',(4.85685941262204,4.06470665762287,5.79648169778678));
#19729=CARTESIAN_POINT('Ctrl Pts',(4.96895273785694,3.51311225847266,5.87204056226937));
#19730=CARTESIAN_POINT('Ctrl Pts',(5.32948706081087,3.08362490768829,5.94730430206206));
#19731=CARTESIAN_POINT('Ctrl Pts',(5.84918345972205,2.88016181192587,6.02222867343336));
#19732=CARTESIAN_POINT('Ctrl Pts',(6.35452293860915,2.94393317727708,6.09058427054729));
#19733=CARTESIAN_POINT('Ctrl Pts',(6.73862464213881,3.18621119370831,6.15244221152227));
#19734=CARTESIAN_POINT('Ctrl Pts',(7.06274421452183,3.62326913030874,6.22636742452222));
#19735=CARTESIAN_POINT('Ctrl Pts',(7.10554518164607,4.18887370461823,6.2998236824497));
#19736=CARTESIAN_POINT('Ctrl Pts',(6.85249430657903,4.66275908350551,6.37276822584886));
#19737=CARTESIAN_POINT('Ctrl Pts',(6.5497353495059,4.92367191327885,6.427214220678));
#19738=CARTESIAN_POINT('Ctrl Pts',(6.17354622005992,5.0548574765238,6.48139179108161));
#19739=CARTESIAN_POINT('Ctrl Pts',(5.71162272614039,5.03777059763326,6.54427708475726));
#19740=CARTESIAN_POINT('Ctrl Pts',(5.24233864535241,4.77825978354709,6.61568154310029));
#19741=CARTESIAN_POINT('Ctrl Pts',(4.95326379832803,4.25369877770726,6.69536188322357));
#19742=CARTESIAN_POINT('Ctrl Pts',(4.9818038280098,3.76014398076512,6.76121462096442));
#19743=CARTESIAN_POINT('Ctrl Pts',(5.15759473503968,3.42113765450785,6.81356035306079));
#19744=CARTESIAN_POINT('Ctrl Pts',(5.37509016478336,3.1909277463555,6.85699607265186));
#19745=CARTESIAN_POINT('Ctrl Pts',(5.68415420144532,3.02775093016466,6.9045368179429));
#19746=CARTESIAN_POINT('Ctrl Pts',(6.06065474879704,2.98556928880557,6.95609988254059));
#19747=CARTESIAN_POINT('Ctrl Pts',(6.48540963358703,3.0992501615105,7.01590966564209));
#19748=CARTESIAN_POINT('Ctrl Pts',(6.86525514523639,3.43902146271441,7.08377076212038));
#19749=CARTESIAN_POINT('Ctrl Pts',(7.02194275655083,3.98577375333824,7.1594543336964));
#19750=CARTESIAN_POINT('Ctrl Pts',(6.86526474012505,4.52718960725205,7.23449044610845));
#19751=CARTESIAN_POINT('Ctrl Pts',(6.44802096899966,4.89921223989767,7.30889435958139));
#19752=CARTESIAN_POINT('Ctrl Pts',(5.90137696830688,4.99143134985884,7.3826856212889));
#19753=CARTESIAN_POINT('Ctrl Pts',(5.3935204403864,4.78042083814242,7.45588715879427));
#19754=CARTESIAN_POINT('Ctrl Pts',(5.07819974972354,4.33501283869676,7.52852550298435));
#19755=CARTESIAN_POINT('Ctrl Pts',(5.04836966910811,3.79411731586998,7.60063046330751));
#19756=CARTESIAN_POINT('Ctrl Pts',(5.3090380544754,3.32352514962416,7.67223501391727));
#19757=CARTESIAN_POINT('Ctrl Pts',(5.77705219363671,3.0653997276032,7.74337509741105));
#19758=CARTESIAN_POINT('Ctrl Pts',(6.30747322592026,3.09561541382198,7.81408939563241));
#19759=CARTESIAN_POINT('Ctrl Pts',(6.73819282943324,3.40169434914954,7.88441910853963));
#19760=CARTESIAN_POINT('Ctrl Pts',(6.93910806394902,3.88763263418749,7.95440767991678));
#19761=CARTESIAN_POINT('Ctrl Pts',(6.85112713024168,4.4038038474583,8.0241006414166));
#19762=CARTESIAN_POINT('Ctrl Pts',(6.50326151996229,4.7926944191776,8.09354511221756));
#19763=CARTESIAN_POINT('Ctrl Pts',(6.00333540186104,4.93653882033147,8.16278997813517));
#19764=CARTESIAN_POINT('Ctrl Pts',(5.50441916176864,4.79271928260646,8.23188457022676));
#19765=CARTESIAN_POINT('Ctrl Pts',(5.17207445064451,4.42041718422104,8.29832531955615));
#19766=CARTESIAN_POINT('Ctrl Pts',(5.07788587706047,3.95400303163662,8.36216766357889));
#19767=CARTESIAN_POINT('Ctrl Pts',(5.21265715790399,3.51770078467468,8.42345990505972));
#19768=CARTESIAN_POINT('Ctrl Pts',(5.51233434006309,3.2251590091176,8.47967535154844));
#19769=CARTESIAN_POINT('Ctrl Pts',(5.86742948238684,3.10120558648341,8.5308308382066));
#19770=CARTESIAN_POINT('Ctrl Pts',(6.20594579383189,3.11370842761258,8.57692529727691));
#19771=CARTESIAN_POINT('Ctrl Pts',(6.51698026701549,3.24945320517786,8.62309340190623));
#19772=CARTESIAN_POINT('Ctrl Pts',(6.75739703043113,3.48976264907366,8.6693433903864));
#19773=CARTESIAN_POINT('Ctrl Pts',(6.89370889027547,3.80199715581543,8.71569298005573));
#19774=CARTESIAN_POINT('Ctrl Pts',(6.90655985977003,4.1432652519204,8.76215627878458));
#19775=CARTESIAN_POINT('Ctrl Pts',(6.79354285202102,4.46653335133218,8.80874733498412));
#19776=CARTESIAN_POINT('Ctrl Pts',(6.5695603815772,4.72695397581073,8.85547977713278));
#19777=CARTESIAN_POINT('Ctrl Pts',(6.26491749594757,4.88808364461752,8.90236695576895));
#19778=CARTESIAN_POINT('Ctrl Pts',(5.92123641980304,4.9269181534952,8.94942165494987));
#19779=CARTESIAN_POINT('Ctrl Pts',(5.5858502843238,4.83717950428668,8.99665654543328));
#19780=CARTESIAN_POINT('Ctrl Pts',(5.30526969819355,4.63026563478705,9.04408310168556));
#19781=CARTESIAN_POINT('Ctrl Pts',(5.11891531372185,4.33392015026218,9.09171390978302));
#19782=CARTESIAN_POINT('Ctrl Pts',(5.05330589123466,3.9883501365582,9.13955739856502));
#19783=CARTESIAN_POINT('Ctrl Pts',(5.11899493172307,3.6412513623554,9.18762957658963));
#19784=CARTESIAN_POINT('Ctrl Pts',(5.32847426937091,3.30689099803783,9.24130025707792));
#19785=CARTESIAN_POINT('Ctrl Pts',(5.69997317447753,3.06648203612493,9.30068647560233));
#19786=CARTESIAN_POINT('Ctrl Pts',(6.18464433636351,3.03002057055539,9.36592638537837));
#19787=CARTESIAN_POINT('Ctrl Pts',(6.64981640514089,3.2391315820987,9.4343725386264));
#19788=CARTESIAN_POINT('Ctrl Pts',(6.96234369156499,3.67816136171562,9.50611611783732));
#19789=CARTESIAN_POINT('Ctrl Pts',(6.99462295056451,4.24181543701733,9.58125450744829));
#19790=CARTESIAN_POINT('Ctrl Pts',(6.71981073272738,4.74045274816967,9.65704281024789));
#19791=CARTESIAN_POINT('Ctrl Pts',(6.21743521044141,5.01890229447707,9.73349236226831));
#19792=CARTESIAN_POINT('Ctrl Pts',(5.63891991598065,4.9871041225948,9.81061030522054));
#19793=CARTESIAN_POINT('Ctrl Pts',(5.16186682104324,4.64948394918386,9.88839996415766));
#19794=CARTESIAN_POINT('Ctrl Pts',(4.9356339179361,4.10514857215579,9.96686064525732));
#19795=CARTESIAN_POINT('Ctrl Pts',(5.03452093290359,3.518955270116,10.0459877096733));
#19796=CARTESIAN_POINT('Ctrl Pts',(5.43342184506395,3.07154769488501,10.1257725741091));
#19797=CARTESIAN_POINT('Ctrl Pts',(6.01387310894385,2.90361920550412,10.2062027693304));
#19798=CARTESIAN_POINT('Ctrl Pts',(6.59922913848389,3.07157463742995,10.2872620089041));
#19799=CARTESIAN_POINT('Ctrl Pts',(7.00853371667816,3.52863910059409,10.3689302828098));
#19800=CARTESIAN_POINT('Ctrl Pts',(7.11263621676139,4.13774647513387,10.4511839831483));
#19801=CARTESIAN_POINT('Ctrl Pts',(6.87508273089367,4.71273794439707,10.5339960578494));
#19802=CARTESIAN_POINT('Ctrl Pts',(6.36477112712681,5.07547594405445,10.617336091636));
#19803=CARTESIAN_POINT('Ctrl Pts',(5.73597718249919,5.11128123267146,10.7011706822485));
#19804=CARTESIAN_POINT('Ctrl Pts',(5.18151627774125,4.80536128072055,10.7854632253289));
#19805=CARTESIAN_POINT('Ctrl Pts',(4.87330818584072,4.24855973184745,10.8701750508535));
#19806=CARTESIAN_POINT('Ctrl Pts',(4.90876847724506,3.61030646882263,10.9552635490111));
#19807=CARTESIAN_POINT('Ctrl Pts',(5.27983677698369,3.08670458823981,11.0406871999814));
#19808=CARTESIAN_POINT('Ctrl Pts',(5.87458924075183,2.84003988052371,11.1263951356316));
#19809=CARTESIAN_POINT('Ctrl Pts',(6.51115887436203,2.94783391493837,11.2123513205601));
#19810=CARTESIAN_POINT('Ctrl Pts',(6.9937846298432,3.3790160528969,11.2984813503604));
#19811=CARTESIAN_POINT('Ctrl Pts',(7.11344785233266,3.79388082621453,11.3560322122809));
#19812=CARTESIAN_POINT('Ctrl Pts',(7.11347588125071,4.00208651046483,11.3847753697116));
#19813=CARTESIAN_POINT('Ctrl Pts',(6.88853591840586,3.99650689970452,2.72519413979724));
#19814=CARTESIAN_POINT('Ctrl Pts',(6.88851341699097,4.16365326312163,2.74826898643115));
#19815=CARTESIAN_POINT('Ctrl Pts',(6.79266132912078,4.49561543834634,2.79432441580812));
#19816=CARTESIAN_POINT('Ctrl Pts',(6.40608079986764,4.84117188888936,2.86333876459104));
#19817=CARTESIAN_POINT('Ctrl Pts',(5.89537064758869,4.92774941819879,2.93229843077413));
#19818=CARTESIAN_POINT('Ctrl Pts',(5.41672830057912,4.72953509189751,3.00126588273576));
#19819=CARTESIAN_POINT('Ctrl Pts',(5.1166250583807,4.306672709096,3.0702877604942));
#19820=CARTESIAN_POINT('Ctrl Pts',(5.08736771323111,3.78819012895638,3.13941747286813));
#19821=CARTESIAN_POINT('Ctrl Pts',(5.33896547323245,3.33253574183947,3.20870462329262));
#19822=CARTESIAN_POINT('Ctrl Pts',(5.79575192905363,3.0797864907763,3.2781993000075));
#19823=CARTESIAN_POINT('Ctrl Pts',(6.31891351953487,3.10885774055101,3.34794975500218));
#19824=CARTESIAN_POINT('Ctrl Pts',(6.74830379130066,3.41309068747734,3.41800297292553));
#19825=CARTESIAN_POINT('Ctrl Pts',(6.9510547607877,3.90154096365469,3.48840404180388));
#19826=CARTESIAN_POINT('Ctrl Pts',(6.86241953458854,4.42589831502308,3.55919606926937));
#19827=CARTESIAN_POINT('Ctrl Pts',(6.50623747712959,4.82517934530622,3.6304197748152));
#19828=CARTESIAN_POINT('Ctrl Pts',(5.98889285076722,4.97476706941445,3.70211342690322));
#19829=CARTESIAN_POINT('Ctrl Pts',(5.46747192638199,4.8251815280753,3.77431232631917));
#19830=CARTESIAN_POINT('Ctrl Pts',(5.11662658985994,4.43315301524721,3.84435526801514));
#19831=CARTESIAN_POINT('Ctrl Pts',(5.0162071016671,3.93768277376914,3.91219951548457));
#19832=CARTESIAN_POINT('Ctrl Pts',(5.15977522500822,3.47058203038587,3.97779639510337));
#19833=CARTESIAN_POINT('Ctrl Pts',(5.51194317996123,3.12652950334333,4.04387582993469));
#19834=CARTESIAN_POINT('Ctrl Pts',(5.98918621922857,2.99147246645262,4.11045074635524));
#19835=CARTESIAN_POINT('Ctrl Pts',(6.47663417367841,3.10248144007294,4.17753425939164));
#19836=CARTESIAN_POINT('Ctrl Pts',(6.82290650696304,3.40770249174057,4.23950079369268));
#19837=CARTESIAN_POINT('Ctrl Pts',(6.98963188577769,3.78984374605777,4.29621647725658));
#19838=CARTESIAN_POINT('Ctrl Pts',(7.00405510461931,4.16689870078161,4.34755696018617));
#19839=CARTESIAN_POINT('Ctrl Pts',(6.87879627909334,4.52513383179102,4.3991953454124));
#19840=CARTESIAN_POINT('Ctrl Pts',(6.60253522883494,4.84705653984927,4.45690236045491));
#19841=CARTESIAN_POINT('Ctrl Pts',(6.16873251221955,5.0432623691803,4.52080477312751));
#19842=CARTESIAN_POINT('Ctrl Pts',(5.64686447947036,5.00445557767878,4.59104407195184));
#19843=CARTESIAN_POINT('Ctrl Pts',(5.24057841000959,4.74254800820931,4.65590513107035));
#19844=CARTESIAN_POINT('Ctrl Pts',(5.00899522734369,4.37323225008896,4.71524515543419));
#19845=CARTESIAN_POINT('Ctrl Pts',(4.90930575929946,3.85626092864323,4.78683239775795));
#19846=CARTESIAN_POINT('Ctrl Pts',(5.16217234267391,3.20584850382231,4.87700824930854));
#19847=CARTESIAN_POINT('Ctrl Pts',(5.92497230789985,2.83677900383088,4.98629122769906));
#19848=CARTESIAN_POINT('Ctrl Pts',(6.74181256947623,3.08741194554306,5.09658083633684));
#19849=CARTESIAN_POINT('Ctrl Pts',(7.17390551165445,3.83314161511176,5.20780897590628));
#19850=CARTESIAN_POINT('Ctrl Pts',(6.9819580933047,4.68005707673005,5.31989205932659));
#19851=CARTESIAN_POINT('Ctrl Pts',(6.25953768149135,5.17368984108256,5.43274490177106));
#19852=CARTESIAN_POINT('Ctrl Pts',(5.58375279011301,5.07190606246186,5.52103398200387));
#19853=CARTESIAN_POINT('Ctrl Pts',(5.2171264186678,4.79260977215518,5.5843153809332));
#19854=CARTESIAN_POINT('Ctrl Pts',(4.98662050379357,4.50455297353126,5.63501958507542));
#19855=CARTESIAN_POINT('Ctrl Pts',(4.84672720555121,4.05225844509292,5.69852705507437));
#19856=CARTESIAN_POINT('Ctrl Pts',(4.95966976348219,3.49436670478253,5.77493252184398));
#19857=CARTESIAN_POINT('Ctrl Pts',(5.32608503302576,3.0571941642239,5.85147820369518));
#19858=CARTESIAN_POINT('Ctrl Pts',(5.8577786092087,2.84858806490979,5.92814817914561));
#19859=CARTESIAN_POINT('Ctrl Pts',(6.37799519612005,2.91385241516062,5.99849589652758));
#19860=CARTESIAN_POINT('Ctrl Pts',(6.77547364153904,3.16436890535246,6.06248319318287));
#19861=CARTESIAN_POINT('Ctrl Pts',(7.11240362358294,3.61827672062001,6.13928266561096));
#19862=CARTESIAN_POINT('Ctrl Pts',(7.15797797270208,4.20949068534465,6.21606342305039));
#19863=CARTESIAN_POINT('Ctrl Pts',(6.89201175633327,4.70809482040669,6.29277578692436));
#19864=CARTESIAN_POINT('Ctrl Pts',(6.5724187217174,4.98368655111803,6.35025944479518));
#19865=CARTESIAN_POINT('Ctrl Pts',(6.17373978783784,5.12287881823028,6.40767588785302));
#19866=CARTESIAN_POINT('Ctrl Pts',(5.6823406060203,5.10487059568676,6.47456829482958));
#19867=CARTESIAN_POINT('Ctrl Pts',(5.18072214992889,4.82794627066138,6.55085129832865));
#19868=CARTESIAN_POINT('Ctrl Pts',(4.86989576148384,4.26483639020975,6.6364092234611));
#19869=CARTESIAN_POINT('Ctrl Pts',(4.90037489921811,3.73231934687877,6.70744530149903));
#19870=CARTESIAN_POINT('Ctrl Pts',(5.09060477626466,3.36533950373994,6.76410150852154));
#19871=CARTESIAN_POINT('Ctrl Pts',(5.32647007599838,3.11562298111662,6.81120994313773));
#19872=CARTESIAN_POINT('Ctrl Pts',(5.66240586094145,2.93816076053336,6.86288601770773));
#19873=CARTESIAN_POINT('Ctrl Pts',(6.07267376915363,2.89210993004352,6.91907319999429));
#19874=CARTESIAN_POINT('Ctrl Pts',(6.53657749618968,3.016168195929,6.98439028889556));
#19875=CARTESIAN_POINT('Ctrl Pts',(6.95258373625134,3.38800637185586,7.05868183418768));
#19876=CARTESIAN_POINT('Ctrl Pts',(7.12475935034317,3.98808875937962,7.14175072442539));
#19877=CARTESIAN_POINT('Ctrl Pts',(6.95257123106385,4.58361106956866,7.22427606622913));
#19878=CARTESIAN_POINT('Ctrl Pts',(6.49303830168486,4.99347016775034,7.30623022342229));
#19879=CARTESIAN_POINT('Ctrl Pts',(5.89034148039216,5.09519412736382,7.38758739392877));
#19880=CARTESIAN_POINT('Ctrl Pts',(5.33019215632419,4.86245516950243,7.46832600555826));
#19881=CARTESIAN_POINT('Ctrl Pts',(4.98251724298352,4.37125724635345,7.54842784023342));
#19882=CARTESIAN_POINT('Ctrl Pts',(4.94974967352826,3.77526621848903,7.62787859492608));
#19883=CARTESIAN_POINT('Ctrl Pts',(5.23669328797984,3.25754942406365,7.70666776492358));
#19884=CARTESIAN_POINT('Ctrl Pts',(5.75070173993439,2.97428478802163,7.78478878417218));
#19885=CARTESIAN_POINT('Ctrl Pts',(6.33159360940416,3.00762384511478,7.86223904300809));
#19886=CARTESIAN_POINT('Ctrl Pts',(6.80161058800981,3.34199006094381,7.93901989429612));
#19887=CARTESIAN_POINT('Ctrl Pts',(7.01978160705851,3.87055260702782,8.01513669056237));
#19888=CARTESIAN_POINT('Ctrl Pts',(6.92415093523139,4.4293210351719,8.09059864737362));
#19889=CARTESIAN_POINT('Ctrl Pts',(6.54909128246045,4.84797549588681,8.16541903687084));
#19890=CARTESIAN_POINT('Ctrl Pts',(6.01337289669146,5.00163880577969,8.23961455650487));
#19891=CARTESIAN_POINT('Ctrl Pts',(5.48221378560674,4.84800085529194,8.31320646706303));
#19892=CARTESIAN_POINT('Ctrl Pts',(5.13096340100248,4.45377036243691,8.38351366750994));
#19893=CARTESIAN_POINT('Ctrl Pts',(5.0323627385332,3.96342516463837,8.45063523838859));
#19894=CARTESIAN_POINT('Ctrl Pts',(5.17348012374935,3.50789656631037,8.51465204594588));
#19895=CARTESIAN_POINT('Ctrl Pts',(5.48462531819063,3.20468646323622,8.5729767503835));
#19896=CARTESIAN_POINT('Ctrl Pts',(5.85082414469273,3.0770670717881,8.6257335694851));
#19897=CARTESIAN_POINT('Ctrl Pts',(6.19802868040939,3.09006779633478,8.67302093640832));
#19898=CARTESIAN_POINT('Ctrl Pts',(6.51524369375132,3.22870235157436,8.72012161242978));
#19899=CARTESIAN_POINT('Ctrl Pts',(6.75904035177302,3.47264584559122,8.76705528956744));
#19900=CARTESIAN_POINT('Ctrl Pts',(6.89641512498249,3.7877651061662,8.81383112604662));
#19901=CARTESIAN_POINT('Ctrl Pts',(6.90913118561134,4.13020988967364,8.8604625749268));
#19902=CARTESIAN_POINT('Ctrl Pts',(6.79618735088614,4.45272948408653,8.90696311627191));
#19903=CARTESIAN_POINT('Ctrl Pts',(6.57378623389393,4.71104075738766,8.95334670323705));
#19904=CARTESIAN_POINT('Ctrl Pts',(6.27305956286147,4.8699014145379,8.99962747923577));
#19905=CARTESIAN_POINT('Ctrl Pts',(5.9357221399501,4.90784517615673,9.04582006230268));
#19906=CARTESIAN_POINT('Ctrl Pts',(5.60836506362981,4.82007977229222,9.09193886304559));
#19907=CARTESIAN_POINT('Ctrl Pts',(5.33601985642346,4.61903031325887,9.13799945638055));
#19908=CARTESIAN_POINT('Ctrl Pts',(5.15614735317848,4.33269414268254,9.18401540712671));
#19909=CARTESIAN_POINT('Ctrl Pts',(5.09325308188048,4.00055596071841,9.23000522886462));
#19910=CARTESIAN_POINT('Ctrl Pts',(5.15620973600908,3.66868476868572,9.27597664931677));
#19911=CARTESIAN_POINT('Ctrl Pts',(5.35571636274036,3.35056367593898,9.32706303832943));
#19912=CARTESIAN_POINT('Ctrl Pts',(5.70751229844252,3.12327742081827,9.38328160753747));
#19913=CARTESIAN_POINT('Ctrl Pts',(6.16358069736592,3.08928682181092,9.44467557644274));
#19914=CARTESIAN_POINT('Ctrl Pts',(6.59876471880261,3.28526401983893,9.50873877884771));
#19915=CARTESIAN_POINT('Ctrl Pts',(6.88933460899203,3.69410126773656,9.57552448067617));
#19916=CARTESIAN_POINT('Ctrl Pts',(6.91885957284284,4.21597246912463,9.64510202690896));
#19917=CARTESIAN_POINT('Ctrl Pts',(6.66534460241342,4.6753100918803,9.71495149050467));
#19918=CARTESIAN_POINT('Ctrl Pts',(6.20418003654574,4.93059951255799,9.78511897981019));
#19919=CARTESIAN_POINT('Ctrl Pts',(5.67516373318628,4.90128602603705,9.85564916097365));
#19920=CARTESIAN_POINT('Ctrl Pts',(5.24030440189317,4.59329235978987,9.92658430072516));
#19921=CARTESIAN_POINT('Ctrl Pts',(5.03464208436496,4.09806935869481,9.99796437337559));
#19922=CARTESIAN_POINT('Ctrl Pts',(5.12454249776034,3.56575273707643,10.0698266715612));
#19923=CARTESIAN_POINT('Ctrl Pts',(5.48643447703374,3.15993632476991,10.1422056370457));
#19924=CARTESIAN_POINT('Ctrl Pts',(6.01271392287784,3.00768903052729,10.2151326458219));
#19925=CARTESIAN_POINT('Ctrl Pts',(6.54349763804324,3.15994780518182,10.2886358327811));
#19926=CARTESIAN_POINT('Ctrl Pts',(6.91494568619907,3.57461636346068,10.362739935582));
#19927=CARTESIAN_POINT('Ctrl Pts',(7.00964422215364,4.12795701399743,10.4374661110181));
#19928=CARTESIAN_POINT('Ctrl Pts',(6.79360471822111,4.65131590326631,10.5128318772436));
#19929=CARTESIAN_POINT('Ctrl Pts',(6.32823247077128,4.98236955691082,10.5888509146754));
#19930=CARTESIAN_POINT('Ctrl Pts',(5.75307679168745,5.01537468552453,10.6655331787411));
#19931=CARTESIAN_POINT('Ctrl Pts',(5.24410756609962,4.7348917526285,10.742884420018));
#19932=CARTESIAN_POINT('Ctrl Pts',(4.95992757920285,4.22219252722917,10.8209071127285));
#19933=CARTESIAN_POINT('Ctrl Pts',(4.99235186719618,3.63187243362919,10.8995983136656));
#19934=CARTESIAN_POINT('Ctrl Pts',(5.33674913990765,3.14520401194109,10.978954454041));
#19935=CARTESIAN_POINT('Ctrl Pts',(5.89179984276686,2.91453821379093,11.0589607383006));
#19936=CARTESIAN_POINT('Ctrl Pts',(6.48919734801473,3.01525134459007,11.1396150305874));
#19937=CARTESIAN_POINT('Ctrl Pts',(6.94487769083775,3.42171931985768,11.2208745171675));
#19938=CARTESIAN_POINT('Ctrl Pts',(7.05870005155304,3.815329029949,11.2754818828969));
#19939=CARTESIAN_POINT('Ctrl Pts',(7.05872671706659,4.01340701081049,11.302826893231));
#19940=CARTESIAN_POINT('Ctrl Pts',(6.95029262135111,3.98586592400863,2.8023339809504));
#19941=CARTESIAN_POINT('Ctrl Pts',(6.95026862138668,4.16414390317928,2.82694556653004));
#19942=CARTESIAN_POINT('Ctrl Pts',(6.84792718615896,4.5177844756354,2.87600736738179));
#19943=CARTESIAN_POINT('Ctrl Pts',(6.43856542568346,4.88296437357288,2.94901039334306));
#19944=CARTESIAN_POINT('Ctrl Pts',(5.9018694632682,4.97345421083968,3.02146390050822));
#19945=CARTESIAN_POINT('Ctrl Pts',(5.40282206296231,4.76616717188768,3.09339167774406));
#19946=CARTESIAN_POINT('Ctrl Pts',(5.09265327923777,4.32810410990818,3.16483096852571));
#19947=CARTESIAN_POINT('Ctrl Pts',(5.06321414551164,3.79557395318726,3.23581733974785));
#19948=CARTESIAN_POINT('Ctrl Pts',(5.32006997075252,3.33168210304646,3.30639105613246));
#19949=CARTESIAN_POINT('Ctrl Pts',(5.78189556541544,3.07685647218943,3.37659389527627));
#19950=CARTESIAN_POINT('Ctrl Pts',(6.306061875331,3.10660643356699,3.44647025580914));
#19951=CARTESIAN_POINT('Ctrl Pts',(6.73237009263218,3.40941104882764,3.51606622649372));
#19952=CARTESIAN_POINT('Ctrl Pts',(6.9316072436104,3.89098016790843,3.58542967826506));
#19953=CARTESIAN_POINT('Ctrl Pts',(6.84438820818325,4.40338817674375,3.6546097587502));
#19954=CARTESIAN_POINT('Ctrl Pts',(6.49860128520392,4.79014614756173,3.7236568258037));
#19955=CARTESIAN_POINT('Ctrl Pts',(6.00070838434377,4.93352949682256,3.79262169707247));
#19956=CARTESIAN_POINT('Ctrl Pts',(5.50293131088009,4.79016627090571,3.86155636785902));
#19957=CARTESIAN_POINT('Ctrl Pts',(5.17063680870318,4.41814039231168,3.92795749478015));
#19958=CARTESIAN_POINT('Ctrl Pts',(5.07636925998576,3.95125665644089,3.99187052042054));
#19959=CARTESIAN_POINT('Ctrl Pts',(5.21117483005849,3.51372127284347,4.05331922475323));
#19960=CARTESIAN_POINT('Ctrl Pts',(5.53960334069174,3.19327535333874,4.11489824654019));
#19961=CARTESIAN_POINT('Ctrl Pts',(5.9823373196834,3.06825891093373,4.17664317907259));
#19962=CARTESIAN_POINT('Ctrl Pts',(6.43241040339628,3.171013191632,4.23858678154593));
#19963=CARTESIAN_POINT('Ctrl Pts',(6.75077514309817,3.45189471835957,4.29557699148632));
#19964=CARTESIAN_POINT('Ctrl Pts',(6.90357262708646,3.8023490484242,4.34758089802266));
#19965=CARTESIAN_POINT('Ctrl Pts',(6.91669227102758,4.14729325868632,4.39454536832608));
#19966=CARTESIAN_POINT('Ctrl Pts',(6.80227826449375,4.47431115711779,4.4416842867902));
#19967=CARTESIAN_POINT('Ctrl Pts',(6.55047858520176,4.76762293520717,4.49426709814841));
#19968=CARTESIAN_POINT('Ctrl Pts',(6.15584183189205,4.94600137762016,4.55239112642174));
#19969=CARTESIAN_POINT('Ctrl Pts',(5.68189599016463,4.91067414241561,4.61618004824093));
#19970=CARTESIAN_POINT('Ctrl Pts',(5.31334944790297,4.67303293352455,4.67501869728126));
#19971=CARTESIAN_POINT('Ctrl Pts',(5.10338347611459,4.33816626959968,4.72882135277698));
#19972=CARTESIAN_POINT('Ctrl Pts',(5.01302782279375,3.86952242328442,4.79371606071519));
#19973=CARTESIAN_POINT('Ctrl Pts',(5.24221807036005,3.27983659742701,4.87546960685059));
#19974=CARTESIAN_POINT('Ctrl Pts',(5.93445578696586,2.94465187737126,4.97466218599338));
#19975=CARTESIAN_POINT('Ctrl Pts',(6.67754359068945,3.17225885927868,5.07498409546016));
#19976=CARTESIAN_POINT('Ctrl Pts',(7.07221058258075,3.85238211276754,5.17647139035252));
#19977=CARTESIAN_POINT('Ctrl Pts',(6.89701951458861,4.62825631875594,5.27914495771684));
#19978=CARTESIAN_POINT('Ctrl Pts',(6.23259905843267,5.0832096411637,5.383014538537));
#19979=CARTESIAN_POINT('Ctrl Pts',(5.60711153340288,4.98967355080173,5.46472964281215));
#19980=CARTESIAN_POINT('Ctrl Pts',(5.2663779085538,4.73018677183093,5.52353337130786));
#19981=CARTESIAN_POINT('Ctrl Pts',(5.05171364146542,4.46199084803395,5.5707490667026));
#19982=CARTESIAN_POINT('Ctrl Pts',(4.92078549467062,4.0395025260862,5.63009241759321));
#19983=CARTESIAN_POINT('Ctrl Pts',(5.02647905426851,3.51580809914182,5.70180650062497));
#19984=CARTESIAN_POINT('Ctrl Pts',(5.37182956432014,3.10326403527445,5.77401633992653));
#19985=CARTESIAN_POINT('Ctrl Pts',(5.87572839886343,2.90518654899726,5.84670063747711));
#19986=CARTESIAN_POINT('Ctrl Pts',(6.37154973362849,2.96705284831529,5.91375284847424));
#19987=CARTESIAN_POINT('Ctrl Pts',(6.75224572110308,3.20681178865771,5.97503021185853));
#19988=CARTESIAN_POINT('Ctrl Pts',(7.07638792235092,3.64307049823467,6.04888072578777));
#19989=CARTESIAN_POINT('Ctrl Pts',(7.12132260031561,4.21508352475279,6.12319600542698));
#19990=CARTESIAN_POINT('Ctrl Pts',(6.86248721959487,4.70093424719145,6.19792697815681));
#19991=CARTESIAN_POINT('Ctrl Pts',(6.54991569820719,4.9706696069471,6.2541726650809));
#19992=CARTESIAN_POINT('Ctrl Pts',(6.15818047323317,5.10763090774658,6.31060524208711));
#19993=CARTESIAN_POINT('Ctrl Pts',(5.67309911779094,5.09006207003428,6.37664509975054));
#19994=CARTESIAN_POINT('Ctrl Pts',(5.17486457479785,4.81560940559756,6.45239362911762));
#19995=CARTESIAN_POINT('Ctrl Pts',(4.86361942238087,4.25305527288563,6.53792585077325));
#19996=CARTESIAN_POINT('Ctrl Pts',(4.89379279366011,3.7170803326296,6.60943330857812));
#19997=CARTESIAN_POINT('Ctrl Pts',(5.08612427336279,3.34581493448056,6.66674534164118));
#19998=CARTESIAN_POINT('Ctrl Pts',(5.32544793519665,3.09232128730982,6.71456119953622));
#19999=CARTESIAN_POINT('Ctrl Pts',(5.66766652291053,2.9113478329744,6.76722272989925));
#20000=CARTESIAN_POINT('Ctrl Pts',(6.08754047418379,2.86404827015208,6.82473109672799));
#20001=CARTESIAN_POINT('Ctrl Pts',(6.56446533915124,2.99137086868677,6.89188059793245));
#20002=CARTESIAN_POINT('Ctrl Pts',(6.9948034795662,3.37532226913545,6.96868485606649));
#20003=CARTESIAN_POINT('Ctrl Pts',(7.17447589821626,3.99939255468548,7.05510703351458));
#20004=CARTESIAN_POINT('Ctrl Pts',(6.99478586305713,4.62290022027637,7.1415001950612));
#20005=CARTESIAN_POINT('Ctrl Pts',(6.51124973729689,5.05490208931216,7.22781058645099));
#20006=CARTESIAN_POINT('Ctrl Pts',(5.87300274454341,5.16315754515052,7.31398823594912));
#20007=CARTESIAN_POINT('Ctrl Pts',(5.27626245766403,4.9157518535826,7.39998244609693));
#20008=CARTESIAN_POINT('Ctrl Pts',(4.90367513413411,4.39016440467849,7.48574424609843));
#20009=CARTESIAN_POINT('Ctrl Pts',(4.86799015684862,3.74901012697494,7.57122574167028));
#20010=CARTESIAN_POINT('Ctrl Pts',(5.17774721687189,3.18930879840211,7.65638083635298));
#20011=CARTESIAN_POINT('Ctrl Pts',(5.73539172659811,2.88158319015515,7.74116527706526));
#20012=CARTESIAN_POINT('Ctrl Pts',(6.36818588209908,2.91757763006315,7.82553703910839));
#20013=CARTESIAN_POINT('Ctrl Pts',(6.88204837896223,3.28278988050203,7.90945652939063));
#20014=CARTESIAN_POINT('Ctrl Pts',(7.12139665456226,3.86203573124861,7.99288684375915));
#20015=CARTESIAN_POINT('Ctrl Pts',(7.01652149023538,4.47596056050852,8.07579394418247));
#20016=CARTESIAN_POINT('Ctrl Pts',(6.60380764727744,4.93686361595779,8.15814694002924));
#20017=CARTESIAN_POINT('Ctrl Pts',(6.01340669994955,5.1063137023791,8.23991814821641));
#20018=CARTESIAN_POINT('Ctrl Pts',(5.42754910994287,4.93690500888135,8.32108351621778));
#20019=CARTESIAN_POINT('Ctrl Pts',(5.04007369566793,4.50201262108148,8.39863925632172));
#20020=CARTESIAN_POINT('Ctrl Pts',(4.93137859155377,3.96129875447802,8.47264958788783));
#20021=CARTESIAN_POINT('Ctrl Pts',(5.08692636002921,3.45942866529189,8.54318005789076));
#20022=CARTESIAN_POINT('Ctrl Pts',(5.42934549869753,3.12585970665682,8.60735193538348));
#20023=CARTESIAN_POINT('Ctrl Pts',(5.83165822285851,2.98571811631052,8.66530492450804));
#20024=CARTESIAN_POINT('Ctrl Pts',(6.21246456474204,3.00003223598118,8.71716377919619));
#20025=CARTESIAN_POINT('Ctrl Pts',(6.55969646693978,3.15186453981375,8.76872368553389));
#20026=CARTESIAN_POINT('Ctrl Pts',(6.8259494531735,3.41838435941792,8.81998539901463));
#20027=CARTESIAN_POINT('Ctrl Pts',(6.9755642780092,3.76179602113988,8.8709503807213));
#20028=CARTESIAN_POINT('Ctrl Pts',(6.98928884168203,4.13394589808556,8.92162065781717));
#20029=CARTESIAN_POINT('Ctrl Pts',(6.86681407627787,4.48337006318172,8.97199922594141));
#20030=CARTESIAN_POINT('Ctrl Pts',(6.62652491520876,4.76228735386696,9.0220897436674));
#20031=CARTESIAN_POINT('Ctrl Pts',(6.30278876416356,4.93316832549157,9.07189671302883));
#20032=CARTESIAN_POINT('Ctrl Pts',(5.94102679899387,4.97373221571464,9.12142526742994));
#20033=CARTESIAN_POINT('Ctrl Pts',(5.59138868673641,4.87985437017635,9.17068149916784));
#20034=CARTESIAN_POINT('Ctrl Pts',(5.30176249967057,4.66587278516982,9.21967172890531));
#20035=CARTESIAN_POINT('Ctrl Pts',(5.11137406242519,4.36251784809578,9.26840406968075));
#20036=CARTESIAN_POINT('Ctrl Pts',(5.04521374956906,4.01229501739208,9.31688487199643));
#20037=CARTESIAN_POINT('Ctrl Pts',(5.11143815667451,3.66404729438246,9.36512665025428));
#20038=CARTESIAN_POINT('Ctrl Pts',(5.31994828225278,3.3319162252874,9.41846785264938));
#20039=CARTESIAN_POINT('Ctrl Pts',(5.68539334341808,3.09625451819029,9.47682673755812));
#20040=CARTESIAN_POINT('Ctrl Pts',(6.15565647977621,3.06162098730779,9.54012238468101));
#20041=CARTESIAN_POINT('Ctrl Pts',(6.60100163878465,3.26265755064533,9.60569449848809));
#20042=CARTESIAN_POINT('Ctrl Pts',(6.89570937301901,3.67833292911367,9.6735261620696));
#20043=CARTESIAN_POINT('Ctrl Pts',(6.92483105663458,4.20415079497554,9.74361163355922));
#20044=CARTESIAN_POINT('Ctrl Pts',(6.67099570698278,4.66278589979716,9.81338629730187));
#20045=CARTESIAN_POINT('Ctrl Pts',(6.21376195556722,4.91519459272152,9.88289707992095));
#20046=CARTESIAN_POINT('Ctrl Pts',(5.69394817961782,4.88578391502196,9.95219218161089));
#20047=CARTESIAN_POINT('Ctrl Pts',(5.2704284246474,4.58509660282537,10.0213211982662));
#20048=CARTESIAN_POINT('Ctrl Pts',(5.07208140876076,4.10599195241877,10.0903346798588));
#20049=CARTESIAN_POINT('Ctrl Pts',(5.15889590488797,3.59526417833319,10.1592839032291));
#20050=CARTESIAN_POINT('Ctrl Pts',(5.50402205104487,3.2090411194233,10.228220499924));
#20051=CARTESIAN_POINT('Ctrl Pts',(6.00199645879297,3.06550206122486,10.2971961924685));
#20052=CARTESIAN_POINT('Ctrl Pts',(6.50067778126696,3.20903914088455,10.36626247131));
#20053=CARTESIAN_POINT('Ctrl Pts',(6.84730300699068,3.59664724321552,10.4354703171584));
#20054=CARTESIAN_POINT('Ctrl Pts',(6.93486943208826,4.11067038305685,10.5048698349302));
#20055=CARTESIAN_POINT('Ctrl Pts',(6.73489012085044,4.59418295967456,10.5745100316563));
#20056=CARTESIAN_POINT('Ctrl Pts',(6.30657877272509,4.89848198644666,10.6444384740937));
#20057=CARTESIAN_POINT('Ctrl Pts',(5.77951424249628,4.92845041178851,10.7147010700453));
#20058=CARTESIAN_POINT('Ctrl Pts',(5.31478041770119,4.67207846115156,10.7853416371438));
#20059=CARTESIAN_POINT('Ctrl Pts',(5.05610819831086,4.20500636751179,10.8564020181706));
#20060=CARTESIAN_POINT('Ctrl Pts',(5.0857236524593,3.66847144880372,10.9279210600486));
#20061=CARTESIAN_POINT('Ctrl Pts',(5.39836096900337,3.22685123457935,10.9999360428456));
#20062=CARTESIAN_POINT('Ctrl Pts',(5.90166701382885,3.01775491662855,11.0724787922852));
#20063=CARTESIAN_POINT('Ctrl Pts',(6.44319411191715,3.10903218763481,11.1455837238297));
#20064=CARTESIAN_POINT('Ctrl Pts',(6.85640687171147,3.47760741146192,11.2192690183675));
#20065=CARTESIAN_POINT('Ctrl Pts',(6.95974821813124,3.83468369063596,11.2688070325982));
#20066=CARTESIAN_POINT('Ctrl Pts',(6.95977245031394,4.01468629256983,11.2936567053819));
#20067=CARTESIAN_POINT('Ctrl Pts',(7.04959553802912,3.98592257196897,2.80202047748269));
#20068=CARTESIAN_POINT('Ctrl Pts',(7.0495690992628,4.18231660611977,2.82913301600999));
#20069=CARTESIAN_POINT('Ctrl Pts',(6.93670763939659,4.57248778363104,2.88326745767727));
#20070=CARTESIAN_POINT('Ctrl Pts',(6.48513783957581,4.97524495721263,2.96379219618304));
#20071=CARTESIAN_POINT('Ctrl Pts',(5.89334453615466,5.07498515734521,3.04369199870337));
#20072=CARTESIAN_POINT('Ctrl Pts',(5.3436674177044,4.84653025539157,3.12292768885556));
#20073=CARTESIAN_POINT('Ctrl Pts',(5.00268894202627,4.364666605717,3.2015021172331));
#20074=CARTESIAN_POINT('Ctrl Pts',(4.97060199746087,3.78028520191834,3.27940497399593));
#20075=CARTESIAN_POINT('Ctrl Pts',(5.25189686376874,3.27280517974582,3.35663745551683));
#20076=CARTESIAN_POINT('Ctrl Pts',(5.75566324646624,2.99519266925544,3.43320128228222));
#20077=CARTESIAN_POINT('Ctrl Pts',(6.32494220199028,3.02785866798993,3.50910361898767));
#20078=CARTESIAN_POINT('Ctrl Pts',(6.78559902355489,3.35554698913419,3.58435484937817));
#20079=CARTESIAN_POINT('Ctrl Pts',(6.99948495517654,3.87366139696321,3.65896947413428));
#20080=CARTESIAN_POINT('Ctrl Pts',(6.9057443504678,4.42157190324475,3.73296568507402));
#20081=CARTESIAN_POINT('Ctrl Pts',(6.53784970235839,4.83229882165359,3.80636524986796));
#20082=CARTESIAN_POINT('Ctrl Pts',(6.0120185388268,4.9831728555397,3.8791937398877));
#20083=CARTESIAN_POINT('Ctrl Pts',(5.49030359434556,4.83232797125952,3.9514794730774));
#20084=CARTESIAN_POINT('Ctrl Pts',(5.14491551233214,4.44480770004393,4.02059711342777));
#20085=CARTESIAN_POINT('Ctrl Pts',(5.0479581811976,3.9623880425108,4.08663861071243));
#20086=CARTESIAN_POINT('Ctrl Pts',(5.18665328053576,3.51366989283078,4.14969046197642));
#20087=CARTESIAN_POINT('Ctrl Pts',(5.52144387908019,3.18760766277227,4.2124195271213));
#20088=CARTESIAN_POINT('Ctrl Pts',(5.96918476728892,3.06163542220108,4.27485533009919));
#20089=CARTESIAN_POINT('Ctrl Pts',(6.42075590052292,3.16517226550806,4.33702918560133));
#20090=CARTESIAN_POINT('Ctrl Pts',(6.73764131916391,3.44527816927544,4.39381653717447));
#20091=CARTESIAN_POINT('Ctrl Pts',(6.88868453992805,3.79220587970527,4.4452957229999));
#20092=CARTESIAN_POINT('Ctrl Pts',(6.9014239480865,4.13174739805484,4.49153188786438));
#20093=CARTESIAN_POINT('Ctrl Pts',(6.78926083467742,4.45182215831981,4.537686425972));
#20094=CARTESIAN_POINT('Ctrl Pts',(6.54392791119181,4.73730781199865,4.58889653940956));
#20095=CARTESIAN_POINT('Ctrl Pts',(6.16188835455284,4.90959837589481,4.64515385611942));
#20096=CARTESIAN_POINT('Ctrl Pts',(5.70642127297529,4.87526922755841,4.70646658352592));
#20097=CARTESIAN_POINT('Ctrl Pts',(5.35472035963564,4.64809143307424,4.76265838587514));
#20098=CARTESIAN_POINT('Ctrl Pts',(5.15549332398101,4.33007449213792,4.81375040542114));
#20099=CARTESIAN_POINT('Ctrl Pts',(5.07028857275984,3.88705211223204,4.87509303555694));
#20100=CARTESIAN_POINT('Ctrl Pts',(5.28634012787146,3.33363343332018,4.95188316018201));
#20101=CARTESIAN_POINT('Ctrl Pts',(5.93164782183758,3.0223131911079,5.04430473366233));
#20102=CARTESIAN_POINT('Ctrl Pts',(6.61875955095355,3.23368682312109,5.13712617207152));
#20103=CARTESIAN_POINT('Ctrl Pts',(6.98100189521977,3.8594139762258,5.23045666115443));
#20104=CARTESIAN_POINT('Ctrl Pts',(6.82012199070105,4.56911642578432,5.32440729336752));
#20105=CARTESIAN_POINT('Ctrl Pts',(6.21438174550616,4.98333168153799,5.41907564338409));
#20106=CARTESIAN_POINT('Ctrl Pts',(5.64601111551489,4.89810409433884,5.49334396077527));
#20107=CARTESIAN_POINT('Ctrl Pts',(5.33675238476666,4.66257985438181,5.54671921479505));
#20108=CARTESIAN_POINT('Ctrl Pts',(5.14200509570064,4.41925435453228,5.58955596074641));
#20109=CARTESIAN_POINT('Ctrl Pts',(5.02329884761106,4.03614199037101,5.6433706981261));
#20110=CARTESIAN_POINT('Ctrl Pts',(5.1191125849183,3.56137279247644,5.70838602410505));
#20111=CARTESIAN_POINT('Ctrl Pts',(5.43225089045909,3.18724975970799,5.77386738846131));
#20112=CARTESIAN_POINT('Ctrl Pts',(5.88948590428537,3.00745078575737,5.8398243456203));
#20113=CARTESIAN_POINT('Ctrl Pts',(6.33993918152939,3.06356712623787,5.90073865605301));
#20114=CARTESIAN_POINT('Ctrl Pts',(6.68630103774357,3.281643012517,5.9564827830694));
#20115=CARTESIAN_POINT('Ctrl Pts',(6.98164902707351,3.67901114045406,6.02376017437336));
#20116=CARTESIAN_POINT('Ctrl Pts',(7.02302073970407,4.20135333823992,6.09162172997393));
#20117=CARTESIAN_POINT('Ctrl Pts',(6.78602411743671,4.64650551718066,6.16007682324628));
#20118=CARTESIAN_POINT('Ctrl Pts',(6.49909070922357,4.89422004985391,6.21171564553496));
#20119=CARTESIAN_POINT('Ctrl Pts',(6.13857069981332,5.02037382723854,6.26365251588237));
#20120=CARTESIAN_POINT('Ctrl Pts',(5.69092255994263,5.0042823319112,6.32459305942612));
#20121=CARTESIAN_POINT('Ctrl Pts',(5.22937221718097,4.75041640031949,6.39473200066671));
#20122=CARTESIAN_POINT('Ctrl Pts',(4.93943560573875,4.2272480207064,6.47429954512901));
#20123=CARTESIAN_POINT('Ctrl Pts',(4.96729044189316,3.72610694101108,6.54114487313096));
#20124=CARTESIAN_POINT('Ctrl Pts',(5.14776765309921,3.37754925528953,6.59494075995518));
#20125=CARTESIAN_POINT('Ctrl Pts',(5.37298367506959,3.13891109087616,6.63994398732567));
#20126=CARTESIAN_POINT('Ctrl Pts',(5.69607229062316,2.96790283821101,6.68966571674888));
#20127=CARTESIAN_POINT('Ctrl Pts',(6.09406846289833,2.92292294668928,6.74417634428119));
#20128=CARTESIAN_POINT('Ctrl Pts',(6.54797103049369,3.04391143962956,6.80807461413231));
#20129=CARTESIAN_POINT('Ctrl Pts',(6.95985684136888,3.4107619087104,6.88151530993674));
#20130=CARTESIAN_POINT('Ctrl Pts',(7.13332472888623,4.01122017583434,6.96467649622193));
#20131=CARTESIAN_POINT('Ctrl Pts',(6.95982343278046,4.61531141611138,7.04834174242524));
#20132=CARTESIAN_POINT('Ctrl Pts',(6.48878339297744,5.03693983688589,7.13247718093113));
#20133=CARTESIAN_POINT('Ctrl Pts',(5.86245106661389,5.14378361000877,7.21704381765844));
#20134=CARTESIAN_POINT('Ctrl Pts',(5.27256413639821,4.89987938398564,7.30200117388622));
#20135=CARTESIAN_POINT('Ctrl Pts',(4.90139038498953,4.3773522928813,7.3873059879696));
#20136=CARTESIAN_POINT('Ctrl Pts',(4.86502821487562,3.73517169107109,7.47291316808673));
#20137=CARTESIAN_POINT('Ctrl Pts',(5.17687462738846,3.17041769901572,7.55877575548064));
#20138=CARTESIAN_POINT('Ctrl Pts',(5.74277715992316,2.85743325263498,7.64484530314035));
#20139=CARTESIAN_POINT('Ctrl Pts',(6.38963489855515,2.89361944545362,7.73107212119948));
#20140=CARTESIAN_POINT('Ctrl Pts',(6.9187191736916,3.26891722683287,7.81740561936278));
#20141=CARTESIAN_POINT('Ctrl Pts',(7.16713887971585,3.86858697286563,7.90379453112234));
#20142=CARTESIAN_POINT('Ctrl Pts',(7.05839689228429,4.50852957543109,7.99018731647296));
#20143=CARTESIAN_POINT('Ctrl Pts',(6.62601310199284,4.99222557577811,8.07653223837689));
#20144=CARTESIAN_POINT('Ctrl Pts',(6.00334857456791,5.17148530967006,8.16277821990696));
#20145=CARTESIAN_POINT('Ctrl Pts',(5.38165839885184,4.9922465523275,8.24887388737063));
#20146=CARTESIAN_POINT('Ctrl Pts',(4.96800443896283,4.52864882133443,8.33158917444569));
#20147=CARTESIAN_POINT('Ctrl Pts',(4.85117478658458,3.94914585502282,8.41090469888688));
#20148=CARTESIAN_POINT('Ctrl Pts',(5.01835098519788,3.4087989648184,8.48682393505967));
#20149=CARTESIAN_POINT('Ctrl Pts',(5.38826105600529,3.04810149166825,8.55617605853122));
#20150=CARTESIAN_POINT('Ctrl Pts',(5.82446178240406,2.89603606129518,8.61900857472436));
#20151=CARTESIAN_POINT('Ctrl Pts',(6.23844478670011,2.9115042535862,8.67538067701557));
#20152=CARTESIAN_POINT('Ctrl Pts',(6.61688532979205,3.07688853253289,8.7315669438026));
#20153=CARTESIAN_POINT('Ctrl Pts',(6.90773379958755,3.36791951130435,8.78755016886496));
#20154=CARTESIAN_POINT('Ctrl Pts',(7.07153121235227,3.74371362143827,8.84332189045714));
#20155=CARTESIAN_POINT('Ctrl Pts',(7.08663687068224,4.15171765258172,8.89887156867244));
#20156=CARTESIAN_POINT('Ctrl Pts',(6.95219592530982,4.53543180820108,8.95418929170758));
#20157=CARTESIAN_POINT('Ctrl Pts',(6.6880103580244,4.84214885063303,9.00926577760877));
#20158=CARTESIAN_POINT('Ctrl Pts',(6.33165270552102,5.03028395831446,9.06409237500585));
#20159=CARTESIAN_POINT('Ctrl Pts',(5.93307245554462,5.07499809321821,9.11866106189048));
#20160=CARTESIAN_POINT('Ctrl Pts',(5.54759924064695,4.97151165964518,9.17296457300614));
#20161=CARTESIAN_POINT('Ctrl Pts',(5.22816739524818,4.73551233569201,9.22699615481349));
#20162=CARTESIAN_POINT('Ctrl Pts',(5.01816475646119,4.40089573947751,9.28075018194062));
#20163=CARTESIAN_POINT('Ctrl Pts',(4.94521345392731,4.01463120053756,9.33422083258747));
#20164=CARTESIAN_POINT('Ctrl Pts',(5.01824316678122,3.63071258185625,9.3874050984931));
#20165=CARTESIAN_POINT('Ctrl Pts',(5.24799706943758,3.26481359843454,9.44617471319816));
#20166=CARTESIAN_POINT('Ctrl Pts',(5.6502251992854,3.00554549082188,9.51040219827145));
#20167=CARTESIAN_POINT('Ctrl Pts',(6.16686070362202,2.96762831361979,9.5799410017488));
#20168=CARTESIAN_POINT('Ctrl Pts',(6.65496938010503,3.18815865352936,9.65182585432177));
#20169=CARTESIAN_POINT('Ctrl Pts',(6.97688124136035,3.64266404253884,9.72597671203471));
#20170=CARTESIAN_POINT('Ctrl Pts',(7.00827068820807,4.2153313758698,9.80231317287426));
#20171=CARTESIAN_POINT('Ctrl Pts',(6.73267428113183,4.71252703931205,9.87799134108143));
#20172=CARTESIAN_POINT('Ctrl Pts',(6.23899646839629,4.98458622955827,9.95302302099409));
#20173=CARTESIAN_POINT('Ctrl Pts',(5.68099320199377,4.95256567160738,10.027423911631));
#20174=CARTESIAN_POINT('Ctrl Pts',(5.22927488560303,4.63126501449131,10.1012134002294));
#20175=CARTESIAN_POINT('Ctrl Pts',(5.01940525157708,4.12297974971796,10.1744145091191));
#20176=CARTESIAN_POINT('Ctrl Pts',(5.11138476437155,3.58510769121428,10.2470537440621));
#20177=CARTESIAN_POINT('Ctrl Pts',(5.47273837574136,3.18157531771205,10.3191609244022));
#20178=CARTESIAN_POINT('Ctrl Pts',(5.98977815820753,3.03315035815018,10.3907690213261));
#20179=CARTESIAN_POINT('Ctrl Pts',(6.50319759533062,3.1815542672455,10.4619139574862));
#20180=CARTESIAN_POINT('Ctrl Pts',(6.85686949607748,3.57795788637289,10.5326344118016));
#20181=CARTESIAN_POINT('Ctrl Pts',(6.94499243867947,4.09891704429121,10.6029715505245));
#20182=CARTESIAN_POINT('Ctrl Pts',(6.74346098168736,4.58456532043327,10.6729688187474));
#20183=CARTESIAN_POINT('Ctrl Pts',(6.31627019450132,4.887312142168,10.7426716956951));
#20184=CARTESIAN_POINT('Ctrl Pts',(5.795341673966,4.91631882842212,10.8121273603339));
#20185=CARTESIAN_POINT('Ctrl Pts',(5.34010223460903,4.66449596467932,10.8813845319597));
#20186=CARTESIAN_POINT('Ctrl Pts',(5.08910582152276,4.21006227233519,10.9504929286156));
#20187=CARTESIAN_POINT('Ctrl Pts',(5.11824740678368,3.69248318848022,11.0195036110717));
#20188=CARTESIAN_POINT('Ctrl Pts',(5.41803510645164,3.26995302498951,11.0884671692244));
#20189=CARTESIAN_POINT('Ctrl Pts',(5.89665777295442,3.07167464695276,11.1574368344658));
#20190=CARTESIAN_POINT('Ctrl Pts',(6.40783698205076,3.15826894639442,11.2264605725725));
#20191=CARTESIAN_POINT('Ctrl Pts',(6.79514811505036,3.50438353372458,11.2955976693271));
#20192=CARTESIAN_POINT('Ctrl Pts',(6.89129494882835,3.83722633847608,11.3417784389734));
#20193=CARTESIAN_POINT('Ctrl Pts',(6.89131751554605,4.00485745751464,11.3649202069907));
#20194=CARTESIAN_POINT('Ctrl Pts',(7.11181267012463,3.99652273239337,2.72529718128223));
#20195=CARTESIAN_POINT('Ctrl Pts',(7.11178468677333,4.20439034555461,2.75399366737857));
#20196=CARTESIAN_POINT('Ctrl Pts',(6.99229223216342,4.61848724239578,2.81144215490518));
#20197=CARTESIAN_POINT('Ctrl Pts',(6.51084510877054,5.04852489640089,2.89735482262377));
#20198=CARTESIAN_POINT('Ctrl Pts',(5.87630191856414,5.15592088469205,2.98303846056107));
#20199=CARTESIAN_POINT('Ctrl Pts',(5.28386722272041,4.91015879874544,3.06841711173038));
#20200=CARTESIAN_POINT('Ctrl Pts',(4.9145125012227,4.38888837216266,3.15345806443366));
#20201=CARTESIAN_POINT('Ctrl Pts',(4.87928389931365,3.75390688897146,3.23811208568559));
#20202=CARTESIAN_POINT('Ctrl Pts',(5.18576872246578,3.20031945302301,3.32234049131729));
#20203=CARTESIAN_POINT('Ctrl Pts',(5.73675947135142,2.89636870787145,3.40610340503253));
#20204=CARTESIAN_POINT('Ctrl Pts',(6.36124760601299,2.93197456969596,3.48936533645486));
#20205=CARTESIAN_POINT('Ctrl Pts',(6.86778482310151,3.29207952654758,3.57209303776967));
#20206=CARTESIAN_POINT('Ctrl Pts',(7.10344047238253,3.8625851317704,3.65425674031009));
#20207=CARTESIAN_POINT('Ctrl Pts',(7.00017622835295,4.46664939122879,3.73582982897195));
#20208=CARTESIAN_POINT('Ctrl Pts',(6.59438164089154,4.91973828380643,3.81678932294849));
#20209=CARTESIAN_POINT('Ctrl Pts',(6.01434996676503,5.08614779432233,3.8971156725437));
#20210=CARTESIAN_POINT('Ctrl Pts',(5.43923281895913,4.91979331284352,3.97679344121952));
#20211=CARTESIAN_POINT('Ctrl Pts',(5.05902725730369,4.49304297642434,4.05288364110645));
#20212=CARTESIAN_POINT('Ctrl Pts',(4.95257325831611,3.96276829797434,4.12546370000634));
#20213=CARTESIAN_POINT('Ctrl Pts',(5.10483091704482,3.47063897988742,4.19460857244748));
#20214=CARTESIAN_POINT('Ctrl Pts',(5.47121169123484,3.11405819360807,4.26322320045));
#20215=CARTESIAN_POINT('Ctrl Pts',(5.95960289303118,2.97684769455774,4.3313087925169));
#20216=CARTESIAN_POINT('Ctrl Pts',(6.45031424924818,3.08960839143403,4.39887090237078));
#20217=CARTESIAN_POINT('Ctrl Pts',(6.79316783996351,3.39296276675552,4.46032401438958));
#20218=CARTESIAN_POINT('Ctrl Pts',(6.95590913286132,3.76709016690528,4.51582256357046));
#20219=CARTESIAN_POINT('Ctrl Pts',(6.96947563984585,4.13190120659762,4.56548949965626));
#20220=CARTESIAN_POINT('Ctrl Pts',(6.84930227955056,4.4744430496678,4.61488140862749));
#20221=CARTESIAN_POINT('Ctrl Pts',(6.58764593315853,4.77868262767437,4.66946120942211));
#20222=CARTESIAN_POINT('Ctrl Pts',(6.18225551372277,4.9611503415574,4.72912558162728));
#20223=CARTESIAN_POINT('Ctrl Pts',(5.70201072840316,4.92457567772025,4.79377016122326));
#20224=CARTESIAN_POINT('Ctrl Pts',(5.33371017211244,4.68624272668883,4.85262925464343));
#20225=CARTESIAN_POINT('Ctrl Pts',(5.12631604517545,4.35485736180581,4.90584700293184));
#20226=CARTESIAN_POINT('Ctrl Pts',(5.03823119748178,3.89554988294405,4.96941983405228));
#20227=CARTESIAN_POINT('Ctrl Pts',(5.26153480425679,3.32684298684606,5.04835443670511));
#20228=CARTESIAN_POINT('Ctrl Pts',(5.91872114617452,3.01150181035348,5.14235135887236));
#20229=CARTESIAN_POINT('Ctrl Pts',(6.60960846454723,3.22564167844968,5.23571236345597));
#20230=CARTESIAN_POINT('Ctrl Pts',(6.9687422296195,3.84900858745817,5.32855016113735));
#20231=CARTESIAN_POINT('Ctrl Pts',(6.80897809494767,4.54707899531827,5.42097218274486));
#20232=CARTESIAN_POINT('Ctrl Pts',(6.2185221854142,4.94907192935034,5.51310245919284));
#20233=CARTESIAN_POINT('Ctrl Pts',(5.67121374043677,4.86595150720937,5.5846135144994));
#20234=CARTESIAN_POINT('Ctrl Pts',(5.37535400789112,4.64052470549437,5.63568594851014));
#20235=CARTESIAN_POINT('Ctrl Pts',(5.18962770820761,4.40837799391791,5.67654309787549));
#20236=CARTESIAN_POINT('Ctrl Pts',(5.07723172202838,4.04462781608614,5.72760987253886));
#20237=CARTESIAN_POINT('Ctrl Pts',(5.1679712265145,3.59672197447019,5.78895382949468));
#20238=CARTESIAN_POINT('Ctrl Pts',(5.46198384079215,3.24594656268194,5.85036986553849));
#20239=CARTESIAN_POINT('Ctrl Pts',(5.88878751737239,3.07843715833668,5.91191699354614));
#20240=CARTESIAN_POINT('Ctrl Pts',(6.30702680268281,3.130800218481,5.96847061746492));
#20241=CARTESIAN_POINT('Ctrl Pts',(6.62732725037718,3.33259493887353,6.02002492173982));
#20242=CARTESIAN_POINT('Ctrl Pts',(6.89953522861249,3.6991031536565,6.08205338958629));
#20243=CARTESIAN_POINT('Ctrl Pts',(6.93707330790287,4.17870591212063,6.14434527738535));
#20244=CARTESIAN_POINT('Ctrl Pts',(6.72016811142097,4.58585169655692,6.20696438244068));
#20245=CARTESIAN_POINT('Ctrl Pts',(6.45817664569874,4.81195395482581,6.25410374705552));
#20246=CARTESIAN_POINT('Ctrl Pts',(6.12962873730158,4.92684991317051,6.30142897812927));
#20247=CARTESIAN_POINT('Ctrl Pts',(5.72233475360488,4.91214713707122,6.35687397377257));
#20248=CARTESIAN_POINT('Ctrl Pts',(5.30311893072218,4.68142574318532,6.4205848471383));
#20249=CARTESIAN_POINT('Ctrl Pts',(5.04016290371371,4.20675760408258,6.49276867761505));
#20250=CARTESIAN_POINT('Ctrl Pts',(5.0654509590544,3.75242640036876,6.55336954181421));
#20251=CARTESIAN_POINT('Ctrl Pts',(5.22905797852052,3.43645099374466,6.60213700890933));
#20252=CARTESIAN_POINT('Ctrl Pts',(5.43324248086317,3.22009850678106,6.64293793377372));
#20253=CARTESIAN_POINT('Ctrl Pts',(5.72623728673697,3.06500752266559,6.68803041467216));
#20254=CARTESIAN_POINT('Ctrl Pts',(6.0873718502829,3.02417318346181,6.73749378609368));
#20255=CARTESIAN_POINT('Ctrl Pts',(6.49958056237668,3.13401391730095,6.79552400870097));
#20256=CARTESIAN_POINT('Ctrl Pts',(6.87420872741322,3.46752510001163,6.86231602845205));
#20257=CARTESIAN_POINT('Ctrl Pts',(7.03246380655118,4.01466143396108,6.9381074668043));
#20258=CARTESIAN_POINT('Ctrl Pts',(6.87415380765172,4.56667427800113,7.01456110403573));
#20259=CARTESIAN_POINT('Ctrl Pts',(6.44261059075647,4.95330475149549,7.09168397047356));
#20260=CARTESIAN_POINT('Ctrl Pts',(5.86656660182286,5.05187894759815,7.16947948898233));
#20261=CARTESIAN_POINT('Ctrl Pts',(5.32169990338654,4.82695809503764,7.24794693879057));
#20262=CARTESIAN_POINT('Ctrl Pts',(4.97712665602631,4.34252758715332,7.32708169022306));
#20263=CARTESIAN_POINT('Ctrl Pts',(4.94283169583294,3.74409201934878,7.40687513104107));
#20264=CARTESIAN_POINT('Ctrl Pts',(5.23454002534415,3.21489657129935,7.48731477307834));
#20265=CARTESIAN_POINT('Ctrl Pts',(5.7672320759956,2.9197426119313,7.56838428888876));
#20266=CARTESIAN_POINT('Ctrl Pts',(6.37987364666838,2.95351657370839,7.65006364226415));
#20267=CARTESIAN_POINT('Ctrl Pts',(6.88421899375099,3.31062599964522,7.73232917532269));
#20268=CARTESIAN_POINT('Ctrl Pts',(7.12283689664109,3.88521461663155,7.81515382444631));
#20269=CARTESIAN_POINT('Ctrl Pts',(7.01849989442465,4.50259033063837,7.89850710335461));
#20270=CARTESIAN_POINT('Ctrl Pts',(6.59915021057424,4.97257211814702,7.98235568954449));
#20271=CARTESIAN_POINT('Ctrl Pts',(5.99079694830932,5.14832315832535,8.06666276416388));
#20272=CARTESIAN_POINT('Ctrl Pts',(5.37898192660989,4.97255939586612,8.15139017469558));
#20273=CARTESIAN_POINT('Ctrl Pts',(4.96880293534666,4.51373060196947,8.23334231554345));
#20274=CARTESIAN_POINT('Ctrl Pts',(4.85189260237043,3.93609133882039,8.31243675137032));
#20275=CARTESIAN_POINT('Ctrl Pts',(5.01914830539027,3.39401212655114,8.38858983618502));
#20276=CARTESIAN_POINT('Ctrl Pts',(5.39213568611697,3.02978414283731,8.45858049946112));
#20277=CARTESIAN_POINT('Ctrl Pts',(5.83456068242697,2.87532762833332,8.52233051921372));
#20278=CARTESIAN_POINT('Ctrl Pts',(6.2563976504673,2.89091867238319,8.57978396734133));
#20279=CARTESIAN_POINT('Ctrl Pts',(6.64379204089303,3.06001729220897,8.6372938912653));
#20280=CARTESIAN_POINT('Ctrl Pts',(6.94291241285394,3.35908198542517,8.69485646707076));
#20281=CARTESIAN_POINT('Ctrl Pts',(7.11219375897664,3.74701895770555,8.75245114097456));
#20282=CARTESIAN_POINT('Ctrl Pts',(7.12802991342669,4.17008904416397,8.81006290988188));
#20283=CARTESIAN_POINT('Ctrl Pts',(6.98819439685561,4.56971599002978,8.86767639059384));
#20284=CARTESIAN_POINT('Ctrl Pts',(6.71207735115476,4.89054230347235,8.92527629676472));
#20285=CARTESIAN_POINT('Ctrl Pts',(6.33801804257999,5.08820852708785,8.98284725480005));
#20286=CARTESIAN_POINT('Ctrl Pts',(5.91791219418438,5.13549865056329,9.04037419115003));
#20287=CARTESIAN_POINT('Ctrl Pts',(5.50999677470214,5.02614912712557,9.09784167989352));
#20288=CARTESIAN_POINT('Ctrl Pts',(5.17064513125212,4.77562145632555,9.15523549031463));
#20289=CARTESIAN_POINT('Ctrl Pts',(4.94667637881517,4.4190272401054,9.21253926230186));
#20290=CARTESIAN_POINT('Ctrl Pts',(4.86850226651354,4.00588978606312,9.26974207914286));
#20291=CARTESIAN_POINT('Ctrl Pts',(4.94674979828523,3.59384604350928,9.32682158908026));
#20292=CARTESIAN_POINT('Ctrl Pts',(5.19398219286077,3.19983307636047,9.39010188193961));
#20293=CARTESIAN_POINT('Ctrl Pts',(5.62842891406782,2.91948832571542,9.45950185374663));
#20294=CARTESIAN_POINT('Ctrl Pts',(6.18870266339045,2.87811165294531,9.53491940251957));
#20295=CARTESIAN_POINT('Ctrl Pts',(6.71997102700817,3.11786770005593,9.61315040836019));
#20296=CARTESIAN_POINT('Ctrl Pts',(7.07166502030134,3.61392112245275,9.69411147936232));
#20297=CARTESIAN_POINT('Ctrl Pts',(7.10629841501347,4.24102436441314,9.77770801648046));
#20298=CARTESIAN_POINT('Ctrl Pts',(6.8039201214026,4.78697294048121,9.86079179520847));
#20299=CARTESIAN_POINT('Ctrl Pts',(6.26092047221784,5.08640170649856,9.94333064976283));
#20300=CARTESIAN_POINT('Ctrl Pts',(5.64615625799004,5.05124065078467,10.0252959694532));
#20301=CARTESIAN_POINT('Ctrl Pts',(5.14798795819423,4.69698307302897,10.1066623869624));
#20302=CARTESIAN_POINT('Ctrl Pts',(4.91645457617,4.13627479051779,10.1874081215893));
#20303=CARTESIAN_POINT('Ctrl Pts',(5.01793256528969,3.5430565390177,10.2675150298338));
#20304=CARTESIAN_POINT('Ctrl Pts',(5.41620966151829,3.09841671767496,10.3469687588456));
#20305=CARTESIAN_POINT('Ctrl Pts',(5.98521736545867,2.9352135316976,10.425758809164));
#20306=CARTESIAN_POINT('Ctrl Pts',(6.54900266284988,3.09836831360138,10.5038786074306));
#20307=CARTESIAN_POINT('Ctrl Pts',(6.93620171362726,3.53270289666941,10.5813255353004));
#20308=CARTESIAN_POINT('Ctrl Pts',(7.03212844521887,4.10149823693161,10.6581009683996));
#20309=CARTESIAN_POINT('Ctrl Pts',(6.81265030124579,4.62953048443375,10.7342102141382));
#20310=CARTESIAN_POINT('Ctrl Pts',(6.34990419138725,4.95701529899763,10.8096625970708));
#20311=CARTESIAN_POINT('Ctrl Pts',(5.78867040436841,4.98785046291451,10.8844711453126));
#20312=CARTESIAN_POINT('Ctrl Pts',(5.30115181038354,4.71765871139221,10.9586530713657));
#20313=CARTESIAN_POINT('Ctrl Pts',(5.03427591020065,4.23348651379917,11.0322284145427));
#20314=CARTESIAN_POINT('Ctrl Pts',(5.06560848410314,3.68591130814391,11.1052227432768));
#20315=CARTESIAN_POINT('Ctrl Pts',(5.38101430423995,3.24226419953413,11.1776606464299));
#20316=CARTESIAN_POINT('Ctrl Pts',(5.880425539423,3.03597565027725,11.2495797762185));
#20317=CARTESIAN_POINT('Ctrl Pts',(6.40940541410578,3.12614693210119,11.320998883741));
#20318=CARTESIAN_POINT('Ctrl Pts',(6.80671016386546,3.48207591472185,11.391988806191));
#20319=CARTESIAN_POINT('Ctrl Pts',(6.904197876148,3.82112270576356,11.4389948979343));
#20320=CARTESIAN_POINT('Ctrl Pts',(6.90422079703474,3.99138467936354,11.4624998600071));
#20321=CARTESIAN_POINT('Ctrl Pts',(7.08935433048845,4.00976795535994,2.62933137786601));
#20322=CARTESIAN_POINT('Ctrl Pts',(7.08932686336054,4.21380092684516,2.65749848499914));
#20323=CARTESIAN_POINT('Ctrl Pts',(6.97222248731657,4.62104874946912,2.71397012399248));
#20324=CARTESIAN_POINT('Ctrl Pts',(6.49589922960142,5.04740557699651,2.79904527326321));
#20325=CARTESIAN_POINT('Ctrl Pts',(5.86337876953338,5.15502662682281,2.88445395646036));
#20326=CARTESIAN_POINT('Ctrl Pts',(5.26845987859067,4.90888461943479,2.97015008062398));
#20327=CARTESIAN_POINT('Ctrl Pts',(4.89468286073338,4.3823824272392,3.05608638842908));
#20328=CARTESIAN_POINT('Ctrl Pts',(4.85824684039757,3.73630572363291,3.14221390254607));
#20329=CARTESIAN_POINT('Ctrl Pts',(5.1716759823261,3.16895431263743,3.22848265655362));
#20330=CARTESIAN_POINT('Ctrl Pts',(5.73951488913489,2.85504085505817,3.31484179770815));
#20331=CARTESIAN_POINT('Ctrl Pts',(6.38760587314015,2.89141605633462,3.4012399391865));
#20332=CARTESIAN_POINT('Ctrl Pts',(6.91689078349781,3.26700626473913,3.48762550541587));
#20333=CARTESIAN_POINT('Ctrl Pts',(7.16497694333469,3.86619302167825,3.57394696350454));
#20334=CARTESIAN_POINT('Ctrl Pts',(7.05635514580648,4.50465829681448,3.66015318410991));
#20335=CARTESIAN_POINT('Ctrl Pts',(6.62546144591164,4.98650451426083,3.74619367966986));
#20336=CARTESIAN_POINT('Ctrl Pts',(6.00586863628371,5.16474080304245,3.83201908797416));
#20337=CARTESIAN_POINT('Ctrl Pts',(5.3881890155353,4.98652307294238,3.91758099817887));
#20338=CARTESIAN_POINT('Ctrl Pts',(4.97772947734064,4.52637645614127,3.99967581713145));
#20339=CARTESIAN_POINT('Ctrl Pts',(4.86215903700014,3.95201587014982,4.07830191834474));
#20340=CARTESIAN_POINT('Ctrl Pts',(5.02745816897514,3.41698964677923,4.15347339544051));
#20341=CARTESIAN_POINT('Ctrl Pts',(5.42685607245378,3.02799004848427,4.22830474934372));
#20342=CARTESIAN_POINT('Ctrl Pts',(5.96089630415468,2.87777906722125,4.30276944214858));
#20343=CARTESIAN_POINT('Ctrl Pts',(6.498883490902,3.00124378734206,4.3768415412266));
#20344=CARTESIAN_POINT('Ctrl Pts',(6.87559304456626,3.33442659112351,4.44436385892624));
#20345=CARTESIAN_POINT('Ctrl Pts',(7.05466837051393,3.74599838952216,4.50542711365477));
#20346=CARTESIAN_POINT('Ctrl Pts',(7.0696349027974,4.14774221788009,4.56013064700762));
#20347=CARTESIAN_POINT('Ctrl Pts',(6.93721352970015,4.5252554236123,4.61457214688294));
#20348=CARTESIAN_POINT('Ctrl Pts',(6.64870709702653,4.86073716900179,4.67476505846687));
#20349=CARTESIAN_POINT('Ctrl Pts',(6.20157167497753,5.06199839012352,4.74058479308716));
#20350=CARTESIAN_POINT('Ctrl Pts',(5.67194776490379,5.02164353040941,4.81188340787891));
#20351=CARTESIAN_POINT('Ctrl Pts',(5.26602157976127,4.75890044535489,4.87677636521827));
#20352=CARTESIAN_POINT('Ctrl Pts',(5.03768164384035,4.39397997563631,4.93538709414076));
#20353=CARTESIAN_POINT('Ctrl Pts',(4.94084027807397,3.88872668946754,5.00532561214801));
#20354=CARTESIAN_POINT('Ctrl Pts',(5.18635472219651,3.26450838263861,5.09201744883042));
#20355=CARTESIAN_POINT('Ctrl Pts',(5.90539913314412,2.9202105403707,5.19484754170443));
#20356=CARTESIAN_POINT('Ctrl Pts',(6.65711372555407,3.15403622799657,5.29649452650138));
#20357=CARTESIAN_POINT('Ctrl Pts',(7.04488820377841,3.82898969542974,5.39697458995052));
#20358=CARTESIAN_POINT('Ctrl Pts',(6.87215114063041,4.57889997706907,5.49632422913287));
#20359=CARTESIAN_POINT('Ctrl Pts',(6.24191793133484,5.00652110364668,5.59458304482695));
#20360=CARTESIAN_POINT('Ctrl Pts',(5.66351128855155,4.91769964682495,5.67021033793647));
#20361=CARTESIAN_POINT('Ctrl Pts',(5.35282932082097,4.68086189098653,5.72386333549739));
#20362=CARTESIAN_POINT('Ctrl Pts',(5.15839756524628,4.43774535650645,5.76664581513995));
#20363=CARTESIAN_POINT('Ctrl Pts',(5.04161323177532,4.05859515840377,5.81987839248399));
#20364=CARTESIAN_POINT('Ctrl Pts',(5.13590711786686,3.59516217764757,5.88336509719667));
#20365=CARTESIAN_POINT('Ctrl Pts',(5.43840686123041,3.23491925336827,5.94650403845761));
#20366=CARTESIAN_POINT('Ctrl Pts',(5.87402874651677,3.06439434962665,6.00930738120382));
#20367=CARTESIAN_POINT('Ctrl Pts',(6.29763282423888,3.11782006164934,6.06660731821252));
#20368=CARTESIAN_POINT('Ctrl Pts',(6.61987707815288,3.32104408260551,6.11849992137742));
#20369=CARTESIAN_POINT('Ctrl Pts',(6.89212340909391,3.68804846399038,6.18058610286788));
#20370=CARTESIAN_POINT('Ctrl Pts',(6.92849012913488,4.16419527438217,6.24242788479418));
#20371=CARTESIAN_POINT('Ctrl Pts',(6.71476440569141,4.56477929198679,6.30407569392624));
#20372=CARTESIAN_POINT('Ctrl Pts',(6.45817356746196,4.78602937621426,6.35022990420567));
#20373=CARTESIAN_POINT('Ctrl Pts',(6.13819352709224,4.89774520806743,6.39631813497738));
#20374=CARTESIAN_POINT('Ctrl Pts',(5.74367658479674,4.88331063715809,6.4500272795765));
#20375=CARTESIAN_POINT('Ctrl Pts',(5.34043473367568,4.66083857309541,6.51135079611151));
#20376=CARTESIAN_POINT('Ctrl Pts',(5.08972251749124,4.20716379117729,6.58030851727006));
#20377=CARTESIAN_POINT('Ctrl Pts',(5.11409780711009,3.77627756908702,6.63779196306467));
#20378=CARTESIAN_POINT('Ctrl Pts',(5.26855297760062,3.47814452242061,6.6838142751157));
#20379=CARTESIAN_POINT('Ctrl Pts',(5.46065965467812,3.27467109759302,6.72219367629874));
#20380=CARTESIAN_POINT('Ctrl Pts',(5.73530920658978,3.12942231351325,6.76445528686445));
#20381=CARTESIAN_POINT('Ctrl Pts',(6.07243948189482,3.09141890367305,6.81062897902484));
#20382=CARTESIAN_POINT('Ctrl Pts',(6.45577255332208,3.19370606878804,6.86459737973638));
#20383=CARTESIAN_POINT('Ctrl Pts',(6.80245632541254,3.50275472411468,6.92643953978416));
#20384=CARTESIAN_POINT('Ctrl Pts',(6.94799187214705,4.00707810157704,6.99628444477559));
#20385=CARTESIAN_POINT('Ctrl Pts',(6.80243463304903,4.51362937231149,7.06644698250257));
#20386=CARTESIAN_POINT('Ctrl Pts',(6.40761680157126,4.86704233480136,7.13697211191855));
#20387=CARTESIAN_POINT('Ctrl Pts',(5.88232251234982,4.95673954752656,7.2079018942272));
#20388=CARTESIAN_POINT('Ctrl Pts',(5.38670220439379,4.75199108710649,7.27927635011301));
#20389=CARTESIAN_POINT('Ctrl Pts',(5.07385848731881,4.311996570288,7.35113272577799));
#20390=CARTESIAN_POINT('Ctrl Pts',(5.04280233204593,3.76912795832174,7.42350548003733));
#20391=CARTESIAN_POINT('Ctrl Pts',(5.30729570140107,3.28932314010225,7.49642597611492));
#20392=CARTESIAN_POINT('Ctrl Pts',(5.79029685260329,3.02166150968425,7.56992236804696));
#20393=CARTESIAN_POINT('Ctrl Pts',(6.34617932999724,3.05222693602592,7.64401937762537));
#20394=CARTESIAN_POINT('Ctrl Pts',(6.80442436050835,3.37654354073427,7.718738186782));
#20395=CARTESIAN_POINT('Ctrl Pts',(7.0217323472939,3.89938565329031,7.79409624897815));
#20396=CARTESIAN_POINT('Ctrl Pts',(6.92676983345605,4.46254487713906,7.87010732284795));
#20397=CARTESIAN_POINT('Ctrl Pts',(6.54339548688279,4.89258459447592,7.94678107889299));
#20398=CARTESIAN_POINT('Ctrl Pts',(5.98523957875296,5.05413538621001,8.02412370189236));
#20399=CARTESIAN_POINT('Ctrl Pts',(5.42166576321615,4.89257860872644,8.10213637984392));
#20400=CARTESIAN_POINT('Ctrl Pts',(5.04208531888007,4.46849204652117,8.1779043724297));
#20401=CARTESIAN_POINT('Ctrl Pts',(4.93322033775504,3.93210456253714,8.25133605036051));
#20402=CARTESIAN_POINT('Ctrl Pts',(5.08894992358947,3.42641889652029,8.32235393730101));
#20403=CARTESIAN_POINT('Ctrl Pts',(5.43819988286549,3.08496270726174,8.3879176883461));
#20404=CARTESIAN_POINT('Ctrl Pts',(5.85439720026083,2.93950036803367,8.44788098607834));
#20405=CARTESIAN_POINT('Ctrl Pts',(6.25273505159805,2.95408037327976,8.50212064403883));
#20406=CARTESIAN_POINT('Ctrl Pts',(6.62002653788648,3.11424812103136,8.55663149134766));
#20407=CARTESIAN_POINT('Ctrl Pts',(6.90478701925602,3.39874133408262,8.61139845473666));
#20408=CARTESIAN_POINT('Ctrl Pts',(7.06667132637044,3.76934455991646,8.66641744103278));
#20409=CARTESIAN_POINT('Ctrl Pts',(7.08202020427562,4.17523803377879,8.72167975629805));
#20410=CARTESIAN_POINT('Ctrl Pts',(6.94744505752561,4.56031046139421,8.77717629140723));
#20411=CARTESIAN_POINT('Ctrl Pts',(6.68040413477401,4.87083756629178,8.83289726235809));
#20412=CARTESIAN_POINT('Ctrl Pts',(6.31698023363933,5.06306852888535,8.88883235968104));
#20413=CARTESIAN_POINT('Ctrl Pts',(5.90695649456619,5.10939104643414,8.94497057613671));
#20414=CARTESIAN_POINT('Ctrl Pts',(5.50700065253343,5.00234857682117,9.00130066835425));
#20415=CARTESIAN_POINT('Ctrl Pts',(5.17271431399361,4.75577353964803,9.05781022196116));
#20416=CARTESIAN_POINT('Ctrl Pts',(4.9510179457879,4.40311243255541,9.11448783483843));
#20417=CARTESIAN_POINT('Ctrl Pts',(4.87316516980905,3.99261893252283,9.17131834442002));
#20418=CARTESIAN_POINT('Ctrl Pts',(4.9511114040548,3.58126083564377,9.22829363176974));
#20419=CARTESIAN_POINT('Ctrl Pts',(5.19884658438153,3.18607396297299,9.29173818490542));
#20420=CARTESIAN_POINT('Ctrl Pts',(5.63659194270646,2.90314131258883,9.36168994453439));
#20421=CARTESIAN_POINT('Ctrl Pts',(6.20478195247466,2.86076221415241,9.43817021297446));
#20422=CARTESIAN_POINT('Ctrl Pts',(6.74696264486986,3.1049657067049,9.51797393250518));
#20423=CARTESIAN_POINT('Ctrl Pts',(7.10847634266124,3.61390080934243,9.60108201071482));
#20424=CARTESIAN_POINT('Ctrl Pts',(7.14484568778978,4.26189538676859,9.68745983808889));
#20425=CARTESIAN_POINT('Ctrl Pts',(6.83086847979655,4.82994556052449,9.77385907953142));
#20426=CARTESIAN_POINT('Ctrl Pts',(6.26290560133959,5.14376668795179,9.86022824454772));
#20427=CARTESIAN_POINT('Ctrl Pts',(5.61567071701958,5.10727846960762,9.94651578749562));
#20428=CARTESIAN_POINT('Ctrl Pts',(5.08788422817577,4.73257952185281,10.0326707962013));
#20429=CARTESIAN_POINT('Ctrl Pts',(4.84092239529325,4.13576460899181,10.1186430740689));
#20430=CARTESIAN_POINT('Ctrl Pts',(4.94909058655262,3.50076872538124,10.204383526189));
#20431=CARTESIAN_POINT('Ctrl Pts',(5.37714970392394,3.02225388968236,10.28984443812));
#20432=CARTESIAN_POINT('Ctrl Pts',(5.99183811975877,2.84554982415397,10.3749797497847));
#20433=CARTESIAN_POINT('Ctrl Pts',(6.60363354102406,3.0222373440814,10.4597453269029));
#20434=CARTESIAN_POINT('Ctrl Pts',(7.02555360958883,3.49505624895605,10.5440992034139));
#20435=CARTESIAN_POINT('Ctrl Pts',(7.13063773339451,4.11653821456178,10.6280018838759));
#20436=CARTESIAN_POINT('Ctrl Pts',(6.89033336017905,4.69526271422283,10.711416501209));
#20437=CARTESIAN_POINT('Ctrl Pts',(6.38213884592012,5.05513174920232,10.7943091108394));
#20438=CARTESIAN_POINT('Ctrl Pts',(5.76451938509553,5.0891965723836,10.876648761637));
#20439=CARTESIAN_POINT('Ctrl Pts',(5.22726652981424,4.79153165150449,10.9584079729608));
#20440=CARTESIAN_POINT('Ctrl Pts',(4.93293862223068,4.25760702694337,11.0395622174635));
#20441=CARTESIAN_POINT('Ctrl Pts',(4.96752800826392,3.65362765488133,11.1200915355985));
#20442=CARTESIAN_POINT('Ctrl Pts',(5.31535928228549,3.1645184205444,11.199977394954));
#20443=CARTESIAN_POINT('Ctrl Pts',(5.86551291199122,2.93739523900251,11.2792100321066));
#20444=CARTESIAN_POINT('Ctrl Pts',(6.44725074043973,3.03673721882636,11.3577722921244));
#20445=CARTESIAN_POINT('Ctrl Pts',(6.88309362092661,3.42739799729367,11.4356761752053));
#20446=CARTESIAN_POINT('Ctrl Pts',(6.98969439584974,3.79852728114815,11.4871433778357));
#20447=CARTESIAN_POINT('Ctrl Pts',(6.98971942206308,3.98442813763357,11.5128073149357));
#20448=CARTESIAN_POINT('Ctrl Pts',(7.02991808875681,4.01367950132643,2.60093950625072));
#20449=CARTESIAN_POINT('Ctrl Pts',(7.02989207675763,4.2069033980654,2.62761440178603));
#20450=CARTESIAN_POINT('Ctrl Pts',(6.91906228277925,4.59266109443473,2.68110100393894));
#20451=CARTESIAN_POINT('Ctrl Pts',(6.46673327264386,4.99790650328683,2.76192471741077));
#20452=CARTESIAN_POINT('Ctrl Pts',(5.86413112095171,5.10068618268087,2.84329382346269));
#20453=CARTESIAN_POINT('Ctrl Pts',(5.29540647873442,4.86571365741625,2.92519940248184));
#20454=CARTESIAN_POINT('Ctrl Pts',(4.93668483059122,4.36097545535027,3.00761016390175));
#20455=CARTESIAN_POINT('Ctrl Pts',(4.9012748009943,3.7391829555439,3.09050047048975));
#20456=CARTESIAN_POINT('Ctrl Pts',(5.20375531414926,3.19090833877407,3.17383809803486));
#20457=CARTESIAN_POINT('Ctrl Pts',(5.75430443912642,2.88613009498686,3.25758993339851));
#20458=CARTESIAN_POINT('Ctrl Pts',(6.38545139705114,2.92117220627119,3.3417196729076));
#20459=CARTESIAN_POINT('Ctrl Pts',(6.90327506386492,3.28814937452449,3.42618914575835));
#20460=CARTESIAN_POINT('Ctrl Pts',(7.14729913444027,3.87647832619913,3.51095806950405));
#20461=CARTESIAN_POINT('Ctrl Pts',(7.0405517643525,4.50636423470096,3.59598432294754));
#20462=CARTESIAN_POINT('Ctrl Pts',(6.6139053462151,4.98408502788234,3.68122453242074));
#20463=CARTESIAN_POINT('Ctrl Pts',(5.99731919977364,5.16189360299918,3.76663340605859));
#20464=CARTESIAN_POINT('Ctrl Pts',(5.3796093434696,4.98411146303029,3.85216606290971));
#20465=CARTESIAN_POINT('Ctrl Pts',(4.96703346331831,4.52220317024434,3.9346029099679));
#20466=CARTESIAN_POINT('Ctrl Pts',(4.85014913796247,3.94288660972667,4.01389923751922));
#20467=CARTESIAN_POINT('Ctrl Pts',(5.01727777754471,3.40093747399747,4.09001126566938));
#20468=CARTESIAN_POINT('Ctrl Pts',(5.42319114007935,3.00520029144226,4.16608362665331));
#20469=CARTESIAN_POINT('Ctrl Pts',(5.96826825075608,2.85157652510321,4.24208401642723));
#20470=CARTESIAN_POINT('Ctrl Pts',(6.51965265029488,2.97784064076311,4.3179783102547));
#20471=CARTESIAN_POINT('Ctrl Pts',(6.90731160615835,3.32036226588665,4.3874112209937));
#20472=CARTESIAN_POINT('Ctrl Pts',(7.09222688286471,3.74505003376669,4.4504132977241));
#20473=CARTESIAN_POINT('Ctrl Pts',(7.10782115128883,4.16075024918538,4.50700494135613));
#20474=CARTESIAN_POINT('Ctrl Pts',(6.97052740566525,4.55245635004197,4.56347583453787));
#20475=CARTESIAN_POINT('Ctrl Pts',(6.67052546791681,4.90147648347343,4.62607046576882));
#20476=CARTESIAN_POINT('Ctrl Pts',(6.20415451901187,5.11161960500053,4.6947175781965));
#20477=CARTESIAN_POINT('Ctrl Pts',(5.64985527632065,5.06959112861472,4.76932506255945));
#20478=CARTESIAN_POINT('Ctrl Pts',(5.22368169854351,4.79395491895654,4.83741708200183));
#20479=CARTESIAN_POINT('Ctrl Pts',(4.98333509090071,4.40998685933077,4.899080077899));
#20480=CARTESIAN_POINT('Ctrl Pts',(4.88112298760244,3.87728182744366,4.97281135437488));
#20481=CARTESIAN_POINT('Ctrl Pts',(5.14030112762427,3.21712419472211,5.0644324068338));
#20482=CARTESIAN_POINT('Ctrl Pts',(5.90290458769374,2.85143281828595,5.17348771964845));
#20483=CARTESIAN_POINT('Ctrl Pts',(6.7026863026727,3.09982654772101,5.28157907216558));
#20484=CARTESIAN_POINT('Ctrl Pts',(7.11632239026351,3.81923483315095,5.38866562056333));
#20485=CARTESIAN_POINT('Ctrl Pts',(6.93207706426345,4.61994543349928,5.49470496192847));
#20486=CARTESIAN_POINT('Ctrl Pts',(6.25865467588588,5.07694576222689,5.59967634800426));
#20487=CARTESIAN_POINT('Ctrl Pts',(5.64053245488443,4.9819883712827,5.68046976345486));
#20488=CARTESIAN_POINT('Ctrl Pts',(5.30862714732133,4.72895402426325,5.73778470389805));
#20489=CARTESIAN_POINT('Ctrl Pts',(5.10096857886021,4.46928837163771,5.78347593827138));
#20490=CARTESIAN_POINT('Ctrl Pts',(4.97635818845021,4.06457032712951,5.84028308812804));
#20491=CARTESIAN_POINT('Ctrl Pts',(5.07699062710392,3.57040680685002,5.90797899550925));
#20492=CARTESIAN_POINT('Ctrl Pts',(5.39917799548324,3.18688187480847,5.9751998496335));
#20493=CARTESIAN_POINT('Ctrl Pts',(5.86231001106952,3.00572140277052,6.04195928029931));
#20494=CARTESIAN_POINT('Ctrl Pts',(6.31166975694251,3.06253707400158,6.10274005594962));
#20495=CARTESIAN_POINT('Ctrl Pts',(6.65277873543009,3.27774270105456,6.15767510739571));
#20496=CARTESIAN_POINT('Ctrl Pts',(6.94036467113044,3.66561745748298,6.22327456672061));
#20497=CARTESIAN_POINT('Ctrl Pts',(6.97826365807328,4.16716906221925,6.28840833804435));
#20498=CARTESIAN_POINT('Ctrl Pts',(6.75385045161079,4.58745250127139,6.35310168841968));
#20499=CARTESIAN_POINT('Ctrl Pts',(6.48522195348155,4.81896893074317,6.40141126646841));
#20500=CARTESIAN_POINT('Ctrl Pts',(6.15118675445815,4.93547873015213,6.44952021848864));
#20501=CARTESIAN_POINT('Ctrl Pts',(5.74056866270979,4.92033083741976,6.50542272631611));
#20502=CARTESIAN_POINT('Ctrl Pts',(5.32259389275759,4.68935725542832,6.56901537249866));
#20503=CARTESIAN_POINT('Ctrl Pts',(5.06421926497528,4.22100075031634,6.64018121519376));
#20504=CARTESIAN_POINT('Ctrl Pts',(5.08957030502715,3.77859543443293,6.69921364506262));
#20505=CARTESIAN_POINT('Ctrl Pts',(5.24759441716036,3.47372752194448,6.7462851377338));
#20506=CARTESIAN_POINT('Ctrl Pts',(5.44359092682464,3.26621147785527,6.78543652559592));
#20507=CARTESIAN_POINT('Ctrl Pts',(5.72292581228413,3.11861363079258,6.82841660268829));
#20508=CARTESIAN_POINT('Ctrl Pts',(6.06449785856132,3.08022887054951,6.87520054940006));
#20509=CARTESIAN_POINT('Ctrl Pts',(6.45141807695574,3.18362516656423,6.92968357040903));
#20510=CARTESIAN_POINT('Ctrl Pts',(6.79954021450763,3.4944566237918,6.99184376751914));
#20511=CARTESIAN_POINT('Ctrl Pts',(6.94455257369293,3.99851035174955,7.06165121796002));
#20512=CARTESIAN_POINT('Ctrl Pts',(6.79951881801366,4.50175945009174,7.13139176275215));
#20513=CARTESIAN_POINT('Ctrl Pts',(6.40906206282621,4.85072232716315,7.20110863853789));
#20514=CARTESIAN_POINT('Ctrl Pts',(5.89265231009902,4.93850009239064,7.27085083928631));
#20515=CARTESIAN_POINT('Ctrl Pts',(5.40816505578386,4.73793399235652,7.34066464993027));
#20516=CARTESIAN_POINT('Ctrl Pts',(5.10409736643278,4.30964140293706,7.41059704735086));
#20517=CARTESIAN_POINT('Ctrl Pts',(5.07438096238868,3.78399512770708,7.480693774379));
#20518=CARTESIAN_POINT('Ctrl Pts',(5.32959988196191,3.32170635411574,7.55099980642353));
#20519=CARTESIAN_POINT('Ctrl Pts',(5.79329351323159,3.06510017082497,7.62155879145399));
#20520=CARTESIAN_POINT('Ctrl Pts',(6.32465269238523,3.09460440832685,7.69241292590983));
#20521=CARTESIAN_POINT('Ctrl Pts',(6.76095436771159,3.40371072785635,7.76360261334252));
#20522=CARTESIAN_POINT('Ctrl Pts',(6.96703348947777,3.90014635488385,7.83516634058253));
#20523=CARTESIAN_POINT('Ctrl Pts',(6.87694103922925,4.43317690107195,7.90714028815697));
#20524=CARTESIAN_POINT('Ctrl Pts',(6.51483692341746,4.83908730724853,7.97955847764587));
#20525=CARTESIAN_POINT('Ctrl Pts',(5.98892532229963,4.9911480385519,8.05245175217812));
#20526=CARTESIAN_POINT('Ctrl Pts',(5.4589113285666,4.83908223472626,8.1258494649861));
#20527=CARTESIAN_POINT('Ctrl Pts',(5.10244841999796,4.44070302191148,8.197037283211));
#20528=CARTESIAN_POINT('Ctrl Pts',(5.00033453276715,3.93733852849481,8.26597109598537));
#20529=CARTESIAN_POINT('Ctrl Pts',(5.14639892975264,3.4630761983191,8.33258741168281));
#20530=CARTESIAN_POINT('Ctrl Pts',(5.47388873341462,3.1429125424487,8.39407540385829));
#20531=CARTESIAN_POINT('Ctrl Pts',(5.8641715122147,3.00649199677749,8.45031883640512));
#20532=CARTESIAN_POINT('Ctrl Pts',(6.23779892120356,3.02015709538156,8.50120513376291));
#20533=CARTESIAN_POINT('Ctrl Pts',(6.58242657954577,3.17041697479611,8.55235638725947));
#20534=CARTESIAN_POINT('Ctrl Pts',(6.84978347686345,3.43748813370884,8.60378217840298));
#20535=CARTESIAN_POINT('Ctrl Pts',(7.0018999972382,3.78564550978687,8.65547994429953));
#20536=CARTESIAN_POINT('Ctrl Pts',(7.01637209912577,4.16729382612512,8.70744988502598));
#20537=CARTESIAN_POINT('Ctrl Pts',(6.88975286292201,4.52974165060038,8.75969157924526));
#20538=CARTESIAN_POINT('Ctrl Pts',(6.63816518893249,4.82237901608623,8.81220378523025));
#20539=CARTESIAN_POINT('Ctrl Pts',(6.29530728381445,5.00379685458895,8.86498461008222));
#20540=CARTESIAN_POINT('Ctrl Pts',(5.90791617233848,5.0476255667439,8.91803141474409));
#20541=CARTESIAN_POINT('Ctrl Pts',(5.52943004553465,4.94639930136838,8.97134091897946));
#20542=CARTESIAN_POINT('Ctrl Pts',(5.21253131321036,4.71274027298687,9.02490904697504));
#20543=CARTESIAN_POINT('Ctrl Pts',(5.00195558202741,4.37791279978642,9.07873127653999));
#20544=CARTESIAN_POINT('Ctrl Pts',(4.92780662503539,3.98740302026396,9.1328019080889));
#20545=CARTESIAN_POINT('Ctrl Pts',(5.00203131662118,3.59525436515709,9.18711575654073));
#20546=CARTESIAN_POINT('Ctrl Pts',(5.23859924290997,3.21769111160157,9.24772564338878));
#20547=CARTESIAN_POINT('Ctrl Pts',(5.6577405937534,2.94654595863672,9.31472306283699));
#20548=CARTESIAN_POINT('Ctrl Pts',(6.2036069027209,2.90560752486482,9.38820031602263));
#20549=CARTESIAN_POINT('Ctrl Pts',(6.72629572804827,3.14075483532117,9.46511861157904));
#20550=CARTESIAN_POINT('Ctrl Pts',(7.07628215733169,3.63287033183077,9.54550944492924));
#20551=CARTESIAN_POINT('Ctrl Pts',(7.11197851063729,4.26218483646211,9.62939466251746));
#20552=CARTESIAN_POINT('Ctrl Pts',(6.80612080116325,4.81633859449139,9.71364494828372));
#20553=CARTESIAN_POINT('Ctrl Pts',(6.25008049897017,5.12402461510688,9.7982215811763));
#20554=CARTESIAN_POINT('Ctrl Pts',(5.6134379987664,5.08853941337726,9.88308356774128));
#20555=CARTESIAN_POINT('Ctrl Pts',(5.09177315554737,4.71869231988539,9.96818842663893));
#20556=CARTESIAN_POINT('Ctrl Pts',(4.84630700308618,4.12658530064136,10.0534921586305));
#20557=CARTESIAN_POINT('Ctrl Pts',(4.95372152652599,3.49350492422017,10.1389496180362));
#20558=CARTESIAN_POINT('Ctrl Pts',(5.38206851630237,3.01403467231803,10.2245147568725));
#20559=CARTESIAN_POINT('Ctrl Pts',(6.00030951953899,2.8358711302214,10.3101408922417));
#20560=CARTESIAN_POINT('Ctrl Pts',(6.61866596499084,3.01401901259021,10.3957809807524));
#20561=CARTESIAN_POINT('Ctrl Pts',(7.04725829779998,3.49369742862853,10.4813878741368));
#20562=CARTESIAN_POINT('Ctrl Pts',(7.15479989009825,4.12729588111062,10.5669146583618));
#20563=CARTESIAN_POINT('Ctrl Pts',(6.90907550905602,4.72009892225302,10.6523148500976));
#20564=CARTESIAN_POINT('Ctrl Pts',(6.38664410339373,5.09051877209641,10.7375427426944));
#20565=CARTESIAN_POINT('Ctrl Pts',(5.74882898183749,5.1260709263418,10.82255355924));
#20566=CARTESIAN_POINT('Ctrl Pts',(5.19158297309713,4.81774319749305,10.9073039912296));
#20567=CARTESIAN_POINT('Ctrl Pts',(4.88491211716783,4.26215901548285,10.9917518139848));
#20568=CARTESIAN_POINT('Ctrl Pts',(4.92071110615179,3.63115782136658,11.0758574895253));
#20569=CARTESIAN_POINT('Ctrl Pts',(5.28508855785184,3.11823615335598,11.1595814256275));
#20570=CARTESIAN_POINT('Ctrl Pts',(5.86358545423481,2.87909939337298,11.2428907919858));
#20571=CARTESIAN_POINT('Ctrl Pts',(6.47726426997602,2.98368077187355,11.3257449258384));
#20572=CARTESIAN_POINT('Ctrl Pts',(6.93842416474904,3.39673555851352,11.4081288318684));
#20573=CARTESIAN_POINT('Ctrl Pts',(7.05150181122087,3.79037870851095,11.4626969504405));
#20574=CARTESIAN_POINT('Ctrl Pts',(7.05152835862377,3.98757933451432,11.489920840408));
#20575=CARTESIAN_POINT('Ctrl Pts',(6.99999815899373,4.01367547347479,2.60093950625072));
#20576=CARTESIAN_POINT('Ctrl Pts',(6.99997288064589,4.20144961727953,2.62686205390015));
#20577=CARTESIAN_POINT('Ctrl Pts',(6.89230845853935,4.57620131355266,2.67882572810781));
#20578=CARTESIAN_POINT('Ctrl Pts',(6.45268902055693,4.97011892113672,2.75738771144581));
#20579=CARTESIAN_POINT('Ctrl Pts',(5.86669155617951,5.07009441973235,2.83651805910941));
#20580=CARTESIAN_POINT('Ctrl Pts',(5.31323924231124,4.84148977638369,2.91622570222972));
#20581=CARTESIAN_POINT('Ctrl Pts',(4.96382442320151,4.34995448969575,2.99649058141579));
#20582=CARTESIAN_POINT('Ctrl Pts',(4.92922815468166,3.74381008719936,3.07730076310524));
#20583=CARTESIAN_POINT('Ctrl Pts',(5.22433988671615,3.20870475874992,3.15863604084508));
#20584=CARTESIAN_POINT('Ctrl Pts',(5.76222017520179,2.91082295270622,3.24047540691231));
#20585=CARTESIAN_POINT('Ctrl Pts',(6.37972244802771,2.94499376197989,3.3227938596108));
#20586=CARTESIAN_POINT('Ctrl Pts',(6.88714214280083,3.30444617999842,3.40556405334158));
#20587=CARTESIAN_POINT('Ctrl Pts',(7.1267179261553,3.88170395597293,3.48875576611263));
#20588=CARTESIAN_POINT('Ctrl Pts',(7.02193956541344,4.50081591971197,3.57233637082151));
#20589=CARTESIAN_POINT('Ctrl Pts',(6.60200309921583,4.97124649007052,3.65627092163634));
#20590=CARTESIAN_POINT('Ctrl Pts',(5.99391816782283,5.1467637293928,3.74052239101179));
#20591=CARTESIAN_POINT('Ctrl Pts',(5.38351410020794,4.97125258500565,3.82505187835831));
#20592=CARTESIAN_POINT('Ctrl Pts',(4.97495278641361,4.51407471129711,3.90667930564871));
#20593=CARTESIAN_POINT('Ctrl Pts',(4.85890493436876,3.9395318134167,3.98533819655606));
#20594=CARTESIAN_POINT('Ctrl Pts',(5.0248445336464,3.40104453051283,4.06097495851984));
#20595=CARTESIAN_POINT('Ctrl Pts',(5.42877344681216,3.00706135834947,4.13670514776413));
#20596=CARTESIAN_POINT('Ctrl Pts',(5.97224138292893,2.85377277882407,4.21249751166765));
#20597=CARTESIAN_POINT('Ctrl Pts',(6.52306794486814,2.97976887786423,4.28832050304671));
#20598=CARTESIAN_POINT('Ctrl Pts',(6.911106619782,3.32248792481664,4.35782394345616));
#20599=CARTESIAN_POINT('Ctrl Pts',(7.09651656274147,3.74815778477591,4.4209850314008));
#20600=CARTESIAN_POINT('Ctrl Pts',(7.11222142726568,4.16541427135673,4.47779829351342));
#20601=CARTESIAN_POINT('Ctrl Pts',(6.97427650626816,4.55914085431083,4.53456660987697));
#20602=CARTESIAN_POINT('Ctrl Pts',(6.6723790417336,4.91046294860728,4.59757802409045));
#20603=CARTESIAN_POINT('Ctrl Pts',(6.20229995228089,5.12240612151564,4.66678931423933));
#20604=CARTESIAN_POINT('Ctrl Pts',(5.6425500433818,5.08009523000915,4.74213609069821));
#20605=CARTESIAN_POINT('Ctrl Pts',(5.21136094690014,4.8013569526932,4.8110335703418));
#20606=CARTESIAN_POINT('Ctrl Pts',(4.96782069609662,4.41239190726546,4.87351124705845));
#20607=CARTESIAN_POINT('Ctrl Pts',(4.86407127402864,3.87207825314686,4.94830807657783));
#20608=CARTESIAN_POINT('Ctrl Pts',(5.12715288076494,3.20107434287668,5.041444793684));
#20609=CARTESIAN_POINT('Ctrl Pts',(5.90376531288412,2.82823955973182,5.15254762811187));
#20610=CARTESIAN_POINT('Ctrl Pts',(6.72029013273465,3.08146453910134,5.2629101070658));
#20611=CARTESIAN_POINT('Ctrl Pts',(7.14364665428008,3.81715099008766,5.37246078991918));
#20612=CARTESIAN_POINT('Ctrl Pts',(6.9551205530812,4.63769652624648,5.4811367937548));
#20613=CARTESIAN_POINT('Ctrl Pts',(6.2641024490546,5.1069317667711,5.5888844628491));
#20614=CARTESIAN_POINT('Ctrl Pts',(5.62881174521816,5.00949357808685,5.67193196549233));
#20615=CARTESIAN_POINT('Ctrl Pts',(5.2874560242671,4.74926815537235,5.73087908447157));
#20616=CARTESIAN_POINT('Ctrl Pts',(5.07381541095866,4.48213637560843,5.77788659685938));
#20617=CARTESIAN_POINT('Ctrl Pts',(4.94552168624609,4.06557538718633,5.83636209008294));
#20618=CARTESIAN_POINT('Ctrl Pts',(5.04911869155687,3.55670415977292,5.90607316299982));
#20619=CARTESIAN_POINT('Ctrl Pts',(5.38099173791495,3.16160536520236,5.97532164753646));
#20620=CARTESIAN_POINT('Ctrl Pts',(5.85816561666817,2.97493727370523,6.04410657341625));
#20621=CARTESIAN_POINT('Ctrl Pts',(6.32119024886796,3.03347138881056,6.1067356435835));
#20622=CARTESIAN_POINT('Ctrl Pts',(6.67264815667528,3.25520245847479,6.16333652453463));
#20623=CARTESIAN_POINT('Ctrl Pts',(6.9689172446974,3.65479400388877,6.23091649769543));
#20624=CARTESIAN_POINT('Ctrl Pts',(7.0079089842411,4.17131843581214,6.29799027327548));
#20625=CARTESIAN_POINT('Ctrl Pts',(6.77691391923214,4.60388596675421,6.36457330679182));
#20626=CARTESIAN_POINT('Ctrl Pts',(6.50054973430609,4.84205531318333,6.414270318429));
#20627=CARTESIAN_POINT('Ctrl Pts',(6.15708960805529,4.96183696463414,6.46373244636263));
#20628=CARTESIAN_POINT('Ctrl Pts',(5.73515865256543,4.94625066250657,6.52117144063107));
#20629=CARTESIAN_POINT('Ctrl Pts',(5.30609465295405,4.70907742816445,6.5864458994691));
#20630=CARTESIAN_POINT('Ctrl Pts',(5.04126574291307,4.22881801076535,6.65940509117474));
#20631=CARTESIAN_POINT('Ctrl Pts',(5.06730780646012,3.7758858483265,6.71983222415362));
#20632=CARTESIAN_POINT('Ctrl Pts',(5.22892555890349,3.46412922360998,6.7679659145206));
#20633=CARTESIAN_POINT('Ctrl Pts',(5.4292015128227,3.25210405867328,6.80796630929891));
#20634=CARTESIAN_POINT('Ctrl Pts',(5.71433691472614,3.10148200562693,6.85183024183257));
#20635=CARTESIAN_POINT('Ctrl Pts',(6.06256514105404,3.06238687711817,6.89952195897341));
#20636=CARTESIAN_POINT('Ctrl Pts',(6.4564976195634,3.16770820022483,6.95498839068538));
#20637=CARTESIAN_POINT('Ctrl Pts',(6.8102288164166,3.48372159458398,7.01814871427154));
#20638=CARTESIAN_POINT('Ctrl Pts',(6.95714247630162,3.9949743218129,7.08893288176131));
#20639=CARTESIAN_POINT('Ctrl Pts',(6.81021696910949,4.50416338125004,7.1594866624322));
#20640=CARTESIAN_POINT('Ctrl Pts',(6.41591912974157,4.85632155826513,7.22985222666365));
#20641=CARTESIAN_POINT('Ctrl Pts',(5.89581150258709,4.9445435848153,7.30007283488175));
#20642=CARTESIAN_POINT('Ctrl Pts',(5.4091541149686,4.74288106481787,7.37019262264602));
#20643=CARTESIAN_POINT('Ctrl Pts',(5.1045916955003,4.31357351873737,7.4402563254929));
#20644=CARTESIAN_POINT('Ctrl Pts',(5.07507074796588,3.78812027671986,7.51030900575102));
#20645=CARTESIAN_POINT('Ctrl Pts',(5.32971571962661,3.32725097083008,7.58039577698861));
#20646=CARTESIAN_POINT('Ctrl Pts',(5.79102376728976,3.07217291555275,7.65056157443439));
#20647=CARTESIAN_POINT('Ctrl Pts',(6.31826217852957,3.10162768020774,7.72085085716367));
#20648=CARTESIAN_POINT('Ctrl Pts',(6.75007083293795,3.40776502742426,7.79130734598018));
#20649=CARTESIAN_POINT('Ctrl Pts',(6.95345754831281,3.89815513784294,7.86197377424134));
#20650=CARTESIAN_POINT('Ctrl Pts',(6.86450758322969,4.42345798565047,7.9328916442996));
#20651=CARTESIAN_POINT('Ctrl Pts',(6.50825373195115,4.82258144361629,8.00410096577401));
#20652=CARTESIAN_POINT('Ctrl Pts',(5.99196133471143,4.97171282731416,8.07564000535001));
#20653=CARTESIAN_POINT('Ctrl Pts',(5.47264846544098,4.82257977354425,8.14754510597589));
#20654=CARTESIAN_POINT('Ctrl Pts',(5.12402089676511,4.43277938176583,8.21717246163365));
#20655=CARTESIAN_POINT('Ctrl Pts',(5.02434526751946,3.94102818280025,8.28449961898673));
#20656=CARTESIAN_POINT('Ctrl Pts',(5.16694197219437,3.47827882962972,8.34949563910625));
#20657=CARTESIAN_POINT('Ctrl Pts',(5.48619587513468,3.16623898773365,8.40942447363167));
#20658=CARTESIAN_POINT('Ctrl Pts',(5.86631955340104,3.03340212556353,8.46419547601151));
#20659=CARTESIAN_POINT('Ctrl Pts',(6.22999033724363,3.04672408117636,8.5137197912885));
#20660=CARTESIAN_POINT('Ctrl Pts',(6.56525962631825,3.19292643023923,8.5634804916257));
#20661=CARTESIAN_POINT('Ctrl Pts',(6.82522778577244,3.45264122124887,8.61348288970028));
#20662=CARTESIAN_POINT('Ctrl Pts',(6.97307814435936,3.7910761621246,8.66373168303779));
#20663=CARTESIAN_POINT('Ctrl Pts',(6.98712736643486,4.16195247500926,8.71423091450252));
#20664=CARTESIAN_POINT('Ctrl Pts',(6.86409623902891,4.5140922960367,8.76498396821101));
#20665=CARTESIAN_POINT('Ctrl Pts',(6.61968565405262,4.79836651831856,8.81599356006379));
#20666=CARTESIAN_POINT('Ctrl Pts',(6.28663324217223,4.97458782653242,8.86726173278701));
#20667=CARTESIAN_POINT('Ctrl Pts',(5.9103163648716,5.01715912899264,8.91878984727219));
#20668=CARTESIAN_POINT('Ctrl Pts',(5.5426151162157,4.91881558382611,8.97057858184767));
#20669=CARTESIAN_POINT('Ctrl Pts',(5.2346932137367,4.69177671709244,9.02262792714338));
#20670=CARTESIAN_POINT('Ctrl Pts',(5.03002927873253,4.36635777160092,9.07493719269484));
#20671=CARTESIAN_POINT('Ctrl Pts',(4.95793528493379,3.98670141138964,9.12750499446544));
#20672=CARTESIAN_POINT('Ctrl Pts',(5.03011221582078,3.60530312678215,9.18032928985668));
#20673=CARTESIAN_POINT('Ctrl Pts',(5.26028491013977,3.23792219176526,9.23930487837506));
#20674=CARTESIAN_POINT('Ctrl Pts',(5.66833767471456,2.97390330572424,9.30453505298122));
#20675=CARTESIAN_POINT('Ctrl Pts',(6.20020835504347,2.93396150339657,9.37613052320119));
#20676=CARTESIAN_POINT('Ctrl Pts',(6.70998344550478,3.16323515745987,9.45115011118038));
#20677=CARTESIAN_POINT('Ctrl Pts',(7.05174463296735,3.64363058779886,9.52964181253653));
#20678=CARTESIAN_POINT('Ctrl Pts',(7.08674491429888,4.25878461683797,9.61164803498578));
#20679=CARTESIAN_POINT('Ctrl Pts',(6.78746221281555,4.80126791369132,9.69412424256602));
#20680=CARTESIAN_POINT('Ctrl Pts',(6.24245359179364,5.10299460367291,9.77704205650278));
#20681=CARTESIAN_POINT('Ctrl Pts',(5.617389337803,5.06829072683056,9.86037045574097));
#20682=CARTESIAN_POINT('Ctrl Pts',(5.10428990247565,4.70469241242162,9.94407602255943));
#20683=CARTESIAN_POINT('Ctrl Pts',(4.86233610468105,4.12145238678417,10.0281230884956));
#20684=CARTESIAN_POINT('Ctrl Pts',(4.96818752346366,3.49664100367693,10.1124739581892));
#20685=CARTESIAN_POINT('Ctrl Pts',(5.39158733307429,3.02246211865203,10.197089152739));
#20686=CARTESIAN_POINT('Ctrl Pts',(6.00398991824946,2.84580444666258,10.2819276236503));
#20687=CARTESIAN_POINT('Ctrl Pts',(6.61780477214459,3.0224619351938,10.3669470022194));
#20688=CARTESIAN_POINT('Ctrl Pts',(7.04420003577297,3.49941215707345,10.4521038303345));
#20689=CARTESIAN_POINT('Ctrl Pts',(7.15155414725,4.13081128487796,10.5373538665558));
#20690=CARTESIAN_POINT('Ctrl Pts',(6.90634183228622,4.72286458915024,10.6226522963591));
#20691=CARTESIAN_POINT('Ctrl Pts',(6.38367034420738,5.09368398946472,10.7079540131199));
#20692=CARTESIAN_POINT('Ctrl Pts',(5.74412845724406,5.12951897848491,10.7932138931513));
#20693=CARTESIAN_POINT('Ctrl Pts',(5.18413119725411,4.81987766303419,10.8783870658711));
#20694=CARTESIAN_POINT('Ctrl Pts',(4.8752129919825,4.26058851376116,10.9634291554075));
#20695=CARTESIAN_POINT('Ctrl Pts',(4.91115871222138,3.62399076997319,11.0482965295163));
#20696=CARTESIAN_POINT('Ctrl Pts',(5.27935908785992,3.10540850794678,11.1329466617017));
#20697=CARTESIAN_POINT('Ctrl Pts',(5.86521072908837,2.86304864268273,11.2173381122335));
#20698=CARTESIAN_POINT('Ctrl Pts',(6.48796989668153,2.969020134583,11.3014313415043));
#20699=CARTESIAN_POINT('Ctrl Pts',(6.95689206969945,3.38875839075872,11.3851878190745));
#20700=CARTESIAN_POINT('Ctrl Pts',(7.07219562678887,3.7896496622666,11.4407823887692));
#20701=CARTESIAN_POINT('Ctrl Pts',(7.07222266979222,3.99053173007441,11.4685145081913));
#20702=CARTESIAN_POINT('',(6.99999815899373,4.01367547347479,2.60093950625072));
#20703=CARTESIAN_POINT('Origin',(7.,4.,2.7));
#20704=CARTESIAN_POINT('',(7.07222266979222,3.99053173007441,11.4685145081913));
#20705=CARTESIAN_POINT('Ctrl Pts',(6.99999815899373,4.01367547347479,2.60093950625072));
#20706=CARTESIAN_POINT('Ctrl Pts',(6.99997288064589,4.20144961727953,2.62686205390015));
#20707=CARTESIAN_POINT('Ctrl Pts',(6.89230845853935,4.57620131355266,2.67882572810781));
#20708=CARTESIAN_POINT('Ctrl Pts',(6.45268902055693,4.97011892113672,2.75738771144581));
#20709=CARTESIAN_POINT('Ctrl Pts',(5.86669155617951,5.07009441973235,2.83651805910941));
#20710=CARTESIAN_POINT('Ctrl Pts',(5.31323924231124,4.84148977638369,2.91622570222972));
#20711=CARTESIAN_POINT('Ctrl Pts',(4.96382442320151,4.34995448969575,2.99649058141579));
#20712=CARTESIAN_POINT('Ctrl Pts',(4.92922815468166,3.74381008719936,3.07730076310524));
#20713=CARTESIAN_POINT('Ctrl Pts',(5.22433988671615,3.20870475874992,3.15863604084508));
#20714=CARTESIAN_POINT('Ctrl Pts',(5.76222017520179,2.91082295270622,3.24047540691231));
#20715=CARTESIAN_POINT('Ctrl Pts',(6.37972244802771,2.94499376197989,3.3227938596108));
#20716=CARTESIAN_POINT('Ctrl Pts',(6.88714214280083,3.30444617999842,3.40556405334158));
#20717=CARTESIAN_POINT('Ctrl Pts',(7.1267179261553,3.88170395597293,3.48875576611263));
#20718=CARTESIAN_POINT('Ctrl Pts',(7.02193956541344,4.50081591971197,3.57233637082151));
#20719=CARTESIAN_POINT('Ctrl Pts',(6.60200309921583,4.97124649007052,3.65627092163634));
#20720=CARTESIAN_POINT('Ctrl Pts',(5.99391816782283,5.1467637293928,3.74052239101179));
#20721=CARTESIAN_POINT('Ctrl Pts',(5.38351410020794,4.97125258500565,3.82505187835831));
#20722=CARTESIAN_POINT('Ctrl Pts',(4.97495278641361,4.51407471129711,3.90667930564871));
#20723=CARTESIAN_POINT('Ctrl Pts',(4.85890493436876,3.9395318134167,3.98533819655606));
#20724=CARTESIAN_POINT('Ctrl Pts',(5.0248445336464,3.40104453051283,4.06097495851984));
#20725=CARTESIAN_POINT('Ctrl Pts',(5.42877344681216,3.00706135834947,4.13670514776413));
#20726=CARTESIAN_POINT('Ctrl Pts',(5.97224138292893,2.85377277882407,4.21249751166765));
#20727=CARTESIAN_POINT('Ctrl Pts',(6.52306794486814,2.97976887786423,4.28832050304671));
#20728=CARTESIAN_POINT('Ctrl Pts',(6.911106619782,3.32248792481664,4.35782394345616));
#20729=CARTESIAN_POINT('Ctrl Pts',(7.09651656274147,3.74815778477591,4.4209850314008));
#20730=CARTESIAN_POINT('Ctrl Pts',(7.11222142726568,4.16541427135673,4.47779829351342));
#20731=CARTESIAN_POINT('Ctrl Pts',(6.97427650626816,4.55914085431083,4.53456660987697));
#20732=CARTESIAN_POINT('Ctrl Pts',(6.6723790417336,4.91046294860728,4.59757802409045));
#20733=CARTESIAN_POINT('Ctrl Pts',(6.20229995228089,5.12240612151564,4.66678931423933));
#20734=CARTESIAN_POINT('Ctrl Pts',(5.6425500433818,5.08009523000915,4.74213609069821));
#20735=CARTESIAN_POINT('Ctrl Pts',(5.21136094690014,4.8013569526932,4.8110335703418));
#20736=CARTESIAN_POINT('Ctrl Pts',(4.96782069609662,4.41239190726546,4.87351124705845));
#20737=CARTESIAN_POINT('Ctrl Pts',(4.86407127402864,3.87207825314686,4.94830807657783));
#20738=CARTESIAN_POINT('Ctrl Pts',(5.12715288076494,3.20107434287668,5.041444793684));
#20739=CARTESIAN_POINT('Ctrl Pts',(5.90376531288412,2.82823955973182,5.15254762811187));
#20740=CARTESIAN_POINT('Ctrl Pts',(6.72029013273465,3.08146453910134,5.2629101070658));
#20741=CARTESIAN_POINT('Ctrl Pts',(7.14364665428008,3.81715099008766,5.37246078991918));
#20742=CARTESIAN_POINT('Ctrl Pts',(6.9551205530812,4.63769652624648,5.4811367937548));
#20743=CARTESIAN_POINT('Ctrl Pts',(6.2641024490546,5.1069317667711,5.5888844628491));
#20744=CARTESIAN_POINT('Ctrl Pts',(5.62881174521816,5.00949357808685,5.67193196549233));
#20745=CARTESIAN_POINT('Ctrl Pts',(5.2874560242671,4.74926815537235,5.73087908447157));
#20746=CARTESIAN_POINT('Ctrl Pts',(5.07381541095866,4.48213637560843,5.77788659685938));
#20747=CARTESIAN_POINT('Ctrl Pts',(4.94552168624609,4.06557538718633,5.83636209008294));
#20748=CARTESIAN_POINT('Ctrl Pts',(5.04911869155687,3.55670415977292,5.90607316299982));
#20749=CARTESIAN_POINT('Ctrl Pts',(5.38099173791495,3.16160536520236,5.97532164753646));
#20750=CARTESIAN_POINT('Ctrl Pts',(5.85816561666817,2.97493727370523,6.04410657341625));
#20751=CARTESIAN_POINT('Ctrl Pts',(6.32119024886796,3.03347138881056,6.1067356435835));
#20752=CARTESIAN_POINT('Ctrl Pts',(6.67264815667528,3.25520245847479,6.16333652453463));
#20753=CARTESIAN_POINT('Ctrl Pts',(6.9689172446974,3.65479400388877,6.23091649769543));
#20754=CARTESIAN_POINT('Ctrl Pts',(7.0079089842411,4.17131843581214,6.29799027327548));
#20755=CARTESIAN_POINT('Ctrl Pts',(6.77691391923214,4.60388596675421,6.36457330679182));
#20756=CARTESIAN_POINT('Ctrl Pts',(6.50054973430609,4.84205531318333,6.414270318429));
#20757=CARTESIAN_POINT('Ctrl Pts',(6.15708960805529,4.96183696463414,6.46373244636263));
#20758=CARTESIAN_POINT('Ctrl Pts',(5.73515865256543,4.94625066250657,6.52117144063107));
#20759=CARTESIAN_POINT('Ctrl Pts',(5.30609465295405,4.70907742816445,6.5864458994691));
#20760=CARTESIAN_POINT('Ctrl Pts',(5.04126574291307,4.22881801076535,6.65940509117474));
#20761=CARTESIAN_POINT('Ctrl Pts',(5.06730780646012,3.7758858483265,6.71983222415362));
#20762=CARTESIAN_POINT('Ctrl Pts',(5.22892555890349,3.46412922360998,6.7679659145206));
#20763=CARTESIAN_POINT('Ctrl Pts',(5.4292015128227,3.25210405867328,6.80796630929891));
#20764=CARTESIAN_POINT('Ctrl Pts',(5.71433691472614,3.10148200562693,6.85183024183257));
#20765=CARTESIAN_POINT('Ctrl Pts',(6.06256514105404,3.06238687711817,6.89952195897341));
#20766=CARTESIAN_POINT('Ctrl Pts',(6.4564976195634,3.16770820022483,6.95498839068538));
#20767=CARTESIAN_POINT('Ctrl Pts',(6.8102288164166,3.48372159458398,7.01814871427154));
#20768=CARTESIAN_POINT('Ctrl Pts',(6.95714247630162,3.9949743218129,7.08893288176131));
#20769=CARTESIAN_POINT('Ctrl Pts',(6.81021696910949,4.50416338125004,7.1594866624322));
#20770=CARTESIAN_POINT('Ctrl Pts',(6.41591912974157,4.85632155826513,7.22985222666365));
#20771=CARTESIAN_POINT('Ctrl Pts',(5.89581150258709,4.9445435848153,7.30007283488175));
#20772=CARTESIAN_POINT('Ctrl Pts',(5.4091541149686,4.74288106481787,7.37019262264602));
#20773=CARTESIAN_POINT('Ctrl Pts',(5.1045916955003,4.31357351873737,7.4402563254929));
#20774=CARTESIAN_POINT('Ctrl Pts',(5.07507074796588,3.78812027671986,7.51030900575102));
#20775=CARTESIAN_POINT('Ctrl Pts',(5.32971571962661,3.32725097083008,7.58039577698861));
#20776=CARTESIAN_POINT('Ctrl Pts',(5.79102376728976,3.07217291555275,7.65056157443439));
#20777=CARTESIAN_POINT('Ctrl Pts',(6.31826217852957,3.10162768020774,7.72085085716367));
#20778=CARTESIAN_POINT('Ctrl Pts',(6.75007083293795,3.40776502742426,7.79130734598018));
#20779=CARTESIAN_POINT('Ctrl Pts',(6.95345754831281,3.89815513784294,7.86197377424134));
#20780=CARTESIAN_POINT('Ctrl Pts',(6.86450758322969,4.42345798565047,7.9328916442996));
#20781=CARTESIAN_POINT('Ctrl Pts',(6.50825373195115,4.82258144361629,8.00410096577401));
#20782=CARTESIAN_POINT('Ctrl Pts',(5.99196133471143,4.97171282731416,8.07564000535001));
#20783=CARTESIAN_POINT('Ctrl Pts',(5.47264846544098,4.82257977354425,8.14754510597589));
#20784=CARTESIAN_POINT('Ctrl Pts',(5.12402089676511,4.43277938176583,8.21717246163365));
#20785=CARTESIAN_POINT('Ctrl Pts',(5.02434526751946,3.94102818280025,8.28449961898673));
#20786=CARTESIAN_POINT('Ctrl Pts',(5.16694197219437,3.47827882962972,8.34949563910625));
#20787=CARTESIAN_POINT('Ctrl Pts',(5.48619587513468,3.16623898773365,8.40942447363167));
#20788=CARTESIAN_POINT('Ctrl Pts',(5.86631955340104,3.03340212556353,8.46419547601151));
#20789=CARTESIAN_POINT('Ctrl Pts',(6.22999033724363,3.04672408117636,8.5137197912885));
#20790=CARTESIAN_POINT('Ctrl Pts',(6.56525962631825,3.19292643023923,8.5634804916257));
#20791=CARTESIAN_POINT('Ctrl Pts',(6.82522778577244,3.45264122124887,8.61348288970028));
#20792=CARTESIAN_POINT('Ctrl Pts',(6.97307814435936,3.7910761621246,8.66373168303779));
#20793=CARTESIAN_POINT('Ctrl Pts',(6.98712736643486,4.16195247500926,8.71423091450252));
#20794=CARTESIAN_POINT('Ctrl Pts',(6.86409623902891,4.5140922960367,8.76498396821101));
#20795=CARTESIAN_POINT('Ctrl Pts',(6.61968565405262,4.79836651831856,8.81599356006379));
#20796=CARTESIAN_POINT('Ctrl Pts',(6.28663324217223,4.97458782653242,8.86726173278701));
#20797=CARTESIAN_POINT('Ctrl Pts',(5.9103163648716,5.01715912899264,8.91878984727219));
#20798=CARTESIAN_POINT('Ctrl Pts',(5.5426151162157,4.91881558382611,8.97057858184767));
#20799=CARTESIAN_POINT('Ctrl Pts',(5.2346932137367,4.69177671709244,9.02262792714338));
#20800=CARTESIAN_POINT('Ctrl Pts',(5.03002927873253,4.36635777160092,9.07493719269484));
#20801=CARTESIAN_POINT('Ctrl Pts',(4.95793528493379,3.98670141138964,9.12750499446544));
#20802=CARTESIAN_POINT('Ctrl Pts',(5.03011221582078,3.60530312678215,9.18032928985668));
#20803=CARTESIAN_POINT('Ctrl Pts',(5.26028491013977,3.23792219176526,9.23930487837506));
#20804=CARTESIAN_POINT('Ctrl Pts',(5.66833767471456,2.97390330572424,9.30453505298122));
#20805=CARTESIAN_POINT('Ctrl Pts',(6.20020835504347,2.93396150339657,9.37613052320119));
#20806=CARTESIAN_POINT('Ctrl Pts',(6.70998344550478,3.16323515745987,9.45115011118038));
#20807=CARTESIAN_POINT('Ctrl Pts',(7.05174463296735,3.64363058779886,9.52964181253653));
#20808=CARTESIAN_POINT('Ctrl Pts',(7.08674491429888,4.25878461683797,9.61164803498578));
#20809=CARTESIAN_POINT('Ctrl Pts',(6.78746221281555,4.80126791369132,9.69412424256602));
#20810=CARTESIAN_POINT('Ctrl Pts',(6.24245359179364,5.10299460367291,9.77704205650278));
#20811=CARTESIAN_POINT('Ctrl Pts',(5.617389337803,5.06829072683056,9.86037045574097));
#20812=CARTESIAN_POINT('Ctrl Pts',(5.10428990247565,4.70469241242162,9.94407602255943));
#20813=CARTESIAN_POINT('Ctrl Pts',(4.86233610468105,4.12145238678417,10.0281230884956));
#20814=CARTESIAN_POINT('Ctrl Pts',(4.96818752346366,3.49664100367693,10.1124739581892));
#20815=CARTESIAN_POINT('Ctrl Pts',(5.39158733307429,3.02246211865203,10.197089152739));
#20816=CARTESIAN_POINT('Ctrl Pts',(6.00398991824946,2.84580444666258,10.2819276236503));
#20817=CARTESIAN_POINT('Ctrl Pts',(6.61780477214459,3.0224619351938,10.3669470022194));
#20818=CARTESIAN_POINT('Ctrl Pts',(7.04420003577297,3.49941215707345,10.4521038303345));
#20819=CARTESIAN_POINT('Ctrl Pts',(7.15155414725,4.13081128487796,10.5373538665558));
#20820=CARTESIAN_POINT('Ctrl Pts',(6.90634183228622,4.72286458915024,10.6226522963591));
#20821=CARTESIAN_POINT('Ctrl Pts',(6.38367034420738,5.09368398946472,10.7079540131199));
#20822=CARTESIAN_POINT('Ctrl Pts',(5.74412845724406,5.12951897848491,10.7932138931513));
#20823=CARTESIAN_POINT('Ctrl Pts',(5.18413119725411,4.81987766303419,10.8783870658711));
#20824=CARTESIAN_POINT('Ctrl Pts',(4.8752129919825,4.26058851376116,10.9634291554075));
#20825=CARTESIAN_POINT('Ctrl Pts',(4.91115871222138,3.62399076997319,11.0482965295163));
#20826=CARTESIAN_POINT('Ctrl Pts',(5.27935908785992,3.10540850794678,11.1329466617017));
#20827=CARTESIAN_POINT('Ctrl Pts',(5.86521072908837,2.86304864268273,11.2173381122335));
#20828=CARTESIAN_POINT('Ctrl Pts',(6.48796989668153,2.969020134583,11.3014313415043));
#20829=CARTESIAN_POINT('Ctrl Pts',(6.95689206969945,3.38875839075872,11.3851878190745));
#20830=CARTESIAN_POINT('Ctrl Pts',(7.07219562678887,3.7896496622666,11.4407823887692));
#20831=CARTESIAN_POINT('Ctrl Pts',(7.07222266979222,3.99053173007441,11.4685145081913));
#20832=CARTESIAN_POINT('Origin',(7.,4.,11.4));
#20833=CARTESIAN_POINT('Origin',(7.,4.,11.4));
#20834=CARTESIAN_POINT('Origin',(7.,4.,2.7));
#20835=CARTESIAN_POINT('',(0.,0.,0.));
#20836=CARTESIAN_POINT('Origin',(1.8,-1.8,0.7));
#20837=CARTESIAN_POINT('',(1.59,-1.8,0.8));
#20838=CARTESIAN_POINT('Origin',(1.8,-1.8,0.8));
#20839=CARTESIAN_POINT('',(1.59,-1.8,2.2));
#20840=CARTESIAN_POINT('',(1.59,-1.8,0.7));
#20841=CARTESIAN_POINT('Origin',(1.8,-1.8,2.2));
#20842=CARTESIAN_POINT('Origin',(1.8,-1.8,2.2));
#20843=CARTESIAN_POINT('Origin',(-1.8,1.8,0.7));
#20844=CARTESIAN_POINT('',(-2.01,1.8,0.8));
#20845=CARTESIAN_POINT('Origin',(-1.8,1.8,0.8));
#20846=CARTESIAN_POINT('',(-2.01,1.8,2.2));
#20847=CARTESIAN_POINT('',(-2.01,1.8,0.7));
#20848=CARTESIAN_POINT('Origin',(-1.8,1.8,2.2));
#20849=CARTESIAN_POINT('Origin',(-1.8,1.8,2.2));
#20850=CARTESIAN_POINT('Origin',(-1.8,-1.8,0.7));
#20851=CARTESIAN_POINT('',(-2.01,-1.8,0.8));
#20852=CARTESIAN_POINT('Origin',(-1.8,-1.8,0.8));
#20853=CARTESIAN_POINT('',(-2.01,-1.8,2.2));
#20854=CARTESIAN_POINT('',(-2.01,-1.8,0.7));
#20855=CARTESIAN_POINT('Origin',(-1.8,-1.8,2.2));
#20856=CARTESIAN_POINT('Origin',(-1.8,-1.8,2.2));
#20857=CARTESIAN_POINT('Origin',(1.8,1.8,0.7));
#20858=CARTESIAN_POINT('',(1.59,1.8,0.8));
#20859=CARTESIAN_POINT('Origin',(1.8,1.8,0.8));
#20860=CARTESIAN_POINT('',(1.59,1.8,2.2));
#20861=CARTESIAN_POINT('',(1.59,1.8,0.7));
#20862=CARTESIAN_POINT('Origin',(1.8,1.8,2.2));
#20863=CARTESIAN_POINT('Origin',(1.8,1.8,2.2));
#20864=CARTESIAN_POINT('Origin',(0.,0.,2.9));
#20865=CARTESIAN_POINT('',(-0.6,-7.34788079488412E-17,2.9));
#20866=CARTESIAN_POINT('Origin',(0.,0.,2.9));
#20867=CARTESIAN_POINT('',(-0.6,7.34788079488412E-17,8.9));
#20868=CARTESIAN_POINT('',(-0.6,-7.34788079488412E-17,2.9));
#20869=CARTESIAN_POINT('Origin',(0.,0.,8.9));
#20870=CARTESIAN_POINT('Origin',(0.,0.,2.9));
#20871=CARTESIAN_POINT('Origin',(0.,0.,8.9));
#20872=CARTESIAN_POINT('',(-0.8,-9.79717439317883E-17,8.9));
#20873=CARTESIAN_POINT('Origin',(0.,0.,8.9));
#20874=CARTESIAN_POINT('',(-0.8,9.79717439317883E-17,10.));
#20875=CARTESIAN_POINT('',(-0.8,-9.79717439317883E-17,8.9));
#20876=CARTESIAN_POINT('Origin',(0.,0.,10.));
#20877=CARTESIAN_POINT('Origin',(0.,0.,8.9));
#20878=CARTESIAN_POINT('Origin',(2.5,2.5,0.8));
#20879=CARTESIAN_POINT('',(2.5,2.5,0.8));
#20880=CARTESIAN_POINT('',(-2.5,2.5,0.8));
#20881=CARTESIAN_POINT('',(2.5,2.5,0.8));
#20882=CARTESIAN_POINT('',(-2.5,2.5,10.));
#20883=CARTESIAN_POINT('',(-2.5,2.5,0.8));
#20884=CARTESIAN_POINT('',(2.5,2.5,10.));
#20885=CARTESIAN_POINT('',(2.5,2.5,10.));
#20886=CARTESIAN_POINT('',(2.5,2.5,0.8));
#20887=CARTESIAN_POINT('Origin',(2.5,-2.5,0.8));
#20888=CARTESIAN_POINT('',(2.5,-2.5,0.8));
#20889=CARTESIAN_POINT('',(2.5,-2.5,0.8));
#20890=CARTESIAN_POINT('',(2.5,-2.5,10.));
#20891=CARTESIAN_POINT('',(2.5,-2.5,10.));
#20892=CARTESIAN_POINT('',(2.5,-2.5,0.8));
#20893=CARTESIAN_POINT('Origin',(-2.5,-2.5,0.8));
#20894=CARTESIAN_POINT('',(-2.5,-2.5,0.8));
#20895=CARTESIAN_POINT('',(-2.5,-2.5,0.8));
#20896=CARTESIAN_POINT('',(-2.5,-2.5,10.));
#20897=CARTESIAN_POINT('',(-2.5,-2.5,10.));
#20898=CARTESIAN_POINT('',(-2.5,-2.5,0.8));
#20899=CARTESIAN_POINT('Origin',(-2.5,2.5,0.8));
#20900=CARTESIAN_POINT('',(-2.5,2.5,0.8));
#20901=CARTESIAN_POINT('',(-2.5,2.5,10.));
#20902=CARTESIAN_POINT('Origin',(0.,0.,10.));
#20903=CARTESIAN_POINT('Origin',(0.,0.,0.8));
#20904=CARTESIAN_POINT('',(0.,0.,0.));
#20905=CARTESIAN_POINT('Origin',(1.8,-1.8,-0.1));
#20906=CARTESIAN_POINT('',(1.525,-1.8,0.));
#20907=CARTESIAN_POINT('Origin',(1.8,-1.8,0.));
#20908=CARTESIAN_POINT('',(1.525,-1.8,0.8));
#20909=CARTESIAN_POINT('',(1.525,-1.8,-0.1));
#20910=CARTESIAN_POINT('Origin',(1.8,-1.8,0.8));
#20911=CARTESIAN_POINT('Origin',(-1.8,1.8,-0.1));
#20912=CARTESIAN_POINT('',(-2.075,1.8,0.));
#20913=CARTESIAN_POINT('Origin',(-1.8,1.8,0.));
#20914=CARTESIAN_POINT('',(-2.075,1.8,0.8));
#20915=CARTESIAN_POINT('',(-2.075,1.8,-0.1));
#20916=CARTESIAN_POINT('Origin',(-1.8,1.8,0.8));
#20917=CARTESIAN_POINT('Origin',(-1.8,-1.8,-0.1));
#20918=CARTESIAN_POINT('',(-2.075,-1.8,0.));
#20919=CARTESIAN_POINT('Origin',(-1.8,-1.8,0.));
#20920=CARTESIAN_POINT('',(-2.075,-1.8,0.8));
#20921=CARTESIAN_POINT('',(-2.075,-1.8,-0.1));
#20922=CARTESIAN_POINT('Origin',(-1.8,-1.8,0.8));
#20923=CARTESIAN_POINT('Origin',(1.8,1.8,-0.1));
#20924=CARTESIAN_POINT('',(1.525,1.8,0.));
#20925=CARTESIAN_POINT('Origin',(1.8,1.8,0.));
#20926=CARTESIAN_POINT('',(1.525,1.8,0.8));
#20927=CARTESIAN_POINT('',(1.525,1.8,-0.1));
#20928=CARTESIAN_POINT('Origin',(1.8,1.8,0.8));
#20929=CARTESIAN_POINT('Origin',(2.9,-2.9,-0.1));
#20930=CARTESIAN_POINT('',(2.625,-2.9,0.));
#20931=CARTESIAN_POINT('Origin',(2.9,-2.9,0.));
#20932=CARTESIAN_POINT('',(2.625,-2.9,0.8));
#20933=CARTESIAN_POINT('',(2.625,-2.9,-0.1));
#20934=CARTESIAN_POINT('Origin',(2.9,-2.9,0.8));
#20935=CARTESIAN_POINT('Origin',(-2.9,2.9,-0.1));
#20936=CARTESIAN_POINT('',(-3.175,2.9,0.));
#20937=CARTESIAN_POINT('Origin',(-2.9,2.9,0.));
#20938=CARTESIAN_POINT('',(-3.175,2.9,0.8));
#20939=CARTESIAN_POINT('',(-3.175,2.9,-0.1));
#20940=CARTESIAN_POINT('Origin',(-2.9,2.9,0.8));
#20941=CARTESIAN_POINT('Origin',(-2.9,-2.9,-0.1));
#20942=CARTESIAN_POINT('',(-3.175,-2.9,0.));
#20943=CARTESIAN_POINT('Origin',(-2.9,-2.9,0.));
#20944=CARTESIAN_POINT('',(-3.175,-2.9,0.8));
#20945=CARTESIAN_POINT('',(-3.175,-2.9,-0.1));
#20946=CARTESIAN_POINT('Origin',(-2.9,-2.9,0.8));
#20947=CARTESIAN_POINT('Origin',(2.9,2.9,-0.1));
#20948=CARTESIAN_POINT('',(2.625,2.9,0.));
#20949=CARTESIAN_POINT('Origin',(2.9,2.9,0.));
#20950=CARTESIAN_POINT('',(2.625,2.9,0.8));
#20951=CARTESIAN_POINT('',(2.625,2.9,-0.1));
#20952=CARTESIAN_POINT('Origin',(2.9,2.9,0.8));
#20953=CARTESIAN_POINT('Origin',(3.5,3.5,0.));
#20954=CARTESIAN_POINT('',(3.5,3.5,0.));
#20955=CARTESIAN_POINT('',(-3.5,3.5,0.));
#20956=CARTESIAN_POINT('',(3.5,3.5,0.));
#20957=CARTESIAN_POINT('',(-3.5,3.5,0.8));
#20958=CARTESIAN_POINT('',(-3.5,3.5,0.));
#20959=CARTESIAN_POINT('',(3.5,3.5,0.8));
#20960=CARTESIAN_POINT('',(3.5,3.5,0.8));
#20961=CARTESIAN_POINT('',(3.5,3.5,0.));
#20962=CARTESIAN_POINT('Origin',(3.5,-3.5,0.));
#20963=CARTESIAN_POINT('',(3.5,-3.5,0.));
#20964=CARTESIAN_POINT('',(3.5,-3.5,0.));
#20965=CARTESIAN_POINT('',(3.5,-3.5,0.8));
#20966=CARTESIAN_POINT('',(3.5,-3.5,0.8));
#20967=CARTESIAN_POINT('',(3.5,-3.5,0.));
#20968=CARTESIAN_POINT('Origin',(-3.5,-3.5,0.));
#20969=CARTESIAN_POINT('',(-3.5,-3.5,0.));
#20970=CARTESIAN_POINT('',(-3.5,-3.5,0.));
#20971=CARTESIAN_POINT('',(-3.5,-3.5,0.8));
#20972=CARTESIAN_POINT('',(-3.5,-3.5,0.8));
#20973=CARTESIAN_POINT('',(-3.5,-3.5,0.));
#20974=CARTESIAN_POINT('Origin',(-3.5,3.5,0.));
#20975=CARTESIAN_POINT('',(-3.5,3.5,0.));
#20976=CARTESIAN_POINT('',(-3.5,3.5,0.8));
#20977=CARTESIAN_POINT('Origin',(0.,0.,0.8));
#20978=CARTESIAN_POINT('Origin',(0.,0.,0.));
#20979=CARTESIAN_POINT('',(0.,0.,0.));
#20980=CARTESIAN_POINT('Origin',(0.,0.,9.));
#20981=CARTESIAN_POINT('',(-0.51,-6.2456986756515E-17,10.));
#20982=CARTESIAN_POINT('Origin',(0.,0.,10.));
#20983=CARTESIAN_POINT('',(-0.51,-6.2456986756515E-17,9.));
#20984=CARTESIAN_POINT('',(-0.51,-6.2456986756515E-17,9.));
#20985=CARTESIAN_POINT('Origin',(0.,0.,9.));
#20986=CARTESIAN_POINT('Origin',(0.,0.,9.));
#20987=CARTESIAN_POINT('',(-0.8,-9.79717439317883E-17,10.));
#20988=CARTESIAN_POINT('Origin',(0.,0.,10.));
#20989=CARTESIAN_POINT('',(-0.8,-9.79717439317883E-17,9.));
#20990=CARTESIAN_POINT('',(-0.8,-9.79717439317883E-17,9.));
#20991=CARTESIAN_POINT('Origin',(0.,0.,9.));
#20992=CARTESIAN_POINT('Origin',(0.,0.,10.));
#20993=CARTESIAN_POINT('Origin',(0.,0.,9.));
#20994=CARTESIAN_POINT('',(0.,0.,0.));
#20995=CARTESIAN_POINT('Origin',(0.,-6.,-0.1));
#20996=CARTESIAN_POINT('',(-0.21,-6.,0.));
#20997=CARTESIAN_POINT('Origin',(0.,-6.,0.));
#20998=CARTESIAN_POINT('',(-0.21,-6.,1.1));
#20999=CARTESIAN_POINT('',(-0.21,-6.,-0.1));
#21000=CARTESIAN_POINT('Origin',(0.,-6.,1.1));
#21001=CARTESIAN_POINT('Origin',(0.,-6.,1.1));
#21002=CARTESIAN_POINT('Origin',(0.,-6.,0.));
#21003=CARTESIAN_POINT('',(-0.5,-6.,13.6));
#21004=CARTESIAN_POINT('Origin',(0.,-6.,13.6));
#21005=CARTESIAN_POINT('',(-0.5,-6.,0.));
#21006=CARTESIAN_POINT('',(-0.5,-6.,0.));
#21007=CARTESIAN_POINT('Origin',(0.,-6.,0.));
#21008=CARTESIAN_POINT('Origin',(0.,-6.,13.6));
#21009=CARTESIAN_POINT('Origin',(0.,-6.,0.));
#21010=CARTESIAN_POINT('',(0.,0.,0.));
#21011=CARTESIAN_POINT('Origin',(0.,-6.,13.6));
#21012=CARTESIAN_POINT('',(-0.5,-6.,14.1));
#21013=CARTESIAN_POINT('Origin',(0.,-6.,14.1));
#21014=CARTESIAN_POINT('',(-0.5,-6.,13.6));
#21015=CARTESIAN_POINT('',(-0.5,-6.,13.6));
#21016=CARTESIAN_POINT('Origin',(0.,-6.,13.6));
#21017=CARTESIAN_POINT('Origin',(0.,-6.,14.1));
#21018=CARTESIAN_POINT('Origin',(0.,-6.,13.6));
#21019=CARTESIAN_POINT('',(0.,0.,0.));
#21020=CARTESIAN_POINT('Origin',(0.,-6.,29.4));
#21021=CARTESIAN_POINT('',(-0.21,-6.,29.4));
#21022=CARTESIAN_POINT('Origin',(0.,-6.,29.4));
#21023=CARTESIAN_POINT('',(-0.21,-6.,30.5));
#21024=CARTESIAN_POINT('',(-0.21,-6.,29.4));
#21025=CARTESIAN_POINT('Origin',(0.,-6.,30.5));
#21026=CARTESIAN_POINT('Origin',(0.,-6.,29.4));
#21027=CARTESIAN_POINT('Origin',(0.,-6.,17.8));
#21028=CARTESIAN_POINT('',(-0.5,-6.,30.5));
#21029=CARTESIAN_POINT('Origin',(0.,-6.,30.5));
#21030=CARTESIAN_POINT('',(-0.5,-6.,17.8));
#21031=CARTESIAN_POINT('',(-0.5,-6.,17.8));
#21032=CARTESIAN_POINT('Origin',(0.,-6.,17.8));
#21033=CARTESIAN_POINT('Origin',(0.,-6.,30.5));
#21034=CARTESIAN_POINT('Origin',(0.,-6.,17.8));
#21035=CARTESIAN_POINT('',(0.,0.,0.));
#21036=CARTESIAN_POINT('Origin',(0.,-6.,17.3));
#21037=CARTESIAN_POINT('',(-0.5,-6.,17.8));
#21038=CARTESIAN_POINT('Origin',(0.,-6.,17.8));
#21039=CARTESIAN_POINT('',(-0.5,-6.,17.3));
#21040=CARTESIAN_POINT('',(-0.5,-6.,17.3));
#21041=CARTESIAN_POINT('Origin',(0.,-6.,17.3));
#21042=CARTESIAN_POINT('Origin',(0.,-6.,17.8));
#21043=CARTESIAN_POINT('Origin',(0.,-6.,17.3));
#21044=CARTESIAN_POINT('',(0.,0.,0.));
#21045=CARTESIAN_POINT('Origin',(0.,6.,-0.1));
#21046=CARTESIAN_POINT('',(-0.21,6.,0.));
#21047=CARTESIAN_POINT('Origin',(0.,6.,0.));
#21048=CARTESIAN_POINT('',(-0.21,6.,1.1));
#21049=CARTESIAN_POINT('',(-0.21,6.,-0.1));
#21050=CARTESIAN_POINT('Origin',(0.,6.,1.1));
#21051=CARTESIAN_POINT('Origin',(0.,6.,1.1));
#21052=CARTESIAN_POINT('Origin',(0.,6.,0.));
#21053=CARTESIAN_POINT('',(-0.5,6.,13.6));
#21054=CARTESIAN_POINT('Origin',(0.,6.,13.6));
#21055=CARTESIAN_POINT('',(-0.5,6.,0.));
#21056=CARTESIAN_POINT('',(-0.5,6.,0.));
#21057=CARTESIAN_POINT('Origin',(0.,6.,0.));
#21058=CARTESIAN_POINT('Origin',(0.,6.,13.6));
#21059=CARTESIAN_POINT('Origin',(0.,6.,0.));
#21060=CARTESIAN_POINT('',(0.,0.,0.));
#21061=CARTESIAN_POINT('Origin',(0.,6.,13.6));
#21062=CARTESIAN_POINT('',(-0.5,6.,14.1));
#21063=CARTESIAN_POINT('Origin',(0.,6.,14.1));
#21064=CARTESIAN_POINT('',(-0.5,6.,13.6));
#21065=CARTESIAN_POINT('',(-0.5,6.,13.6));
#21066=CARTESIAN_POINT('Origin',(0.,6.,13.6));
#21067=CARTESIAN_POINT('Origin',(0.,6.,14.1));
#21068=CARTESIAN_POINT('Origin',(0.,6.,13.6));
#21069=CARTESIAN_POINT('',(0.,0.,0.));
#21070=CARTESIAN_POINT('Origin',(0.,6.,29.4));
#21071=CARTESIAN_POINT('',(-0.21,6.,29.4));
#21072=CARTESIAN_POINT('Origin',(0.,6.,29.4));
#21073=CARTESIAN_POINT('',(-0.21,6.,30.5));
#21074=CARTESIAN_POINT('',(-0.21,6.,29.4));
#21075=CARTESIAN_POINT('Origin',(0.,6.,30.5));
#21076=CARTESIAN_POINT('Origin',(0.,6.,29.4));
#21077=CARTESIAN_POINT('Origin',(0.,6.,17.8));
#21078=CARTESIAN_POINT('',(-0.5,6.,30.5));
#21079=CARTESIAN_POINT('Origin',(0.,6.,30.5));
#21080=CARTESIAN_POINT('',(-0.5,6.,17.8));
#21081=CARTESIAN_POINT('',(-0.5,6.,17.8));
#21082=CARTESIAN_POINT('Origin',(0.,6.,17.8));
#21083=CARTESIAN_POINT('Origin',(0.,6.,30.5));
#21084=CARTESIAN_POINT('Origin',(0.,6.,17.8));
#21085=CARTESIAN_POINT('',(0.,0.,0.));
#21086=CARTESIAN_POINT('Origin',(0.,6.,17.3));
#21087=CARTESIAN_POINT('',(-0.5,6.,17.8));
#21088=CARTESIAN_POINT('Origin',(0.,6.,17.8));
#21089=CARTESIAN_POINT('',(-0.5,6.,17.3));
#21090=CARTESIAN_POINT('',(-0.5,6.,17.3));
#21091=CARTESIAN_POINT('Origin',(0.,6.,17.3));
#21092=CARTESIAN_POINT('Origin',(0.,6.,17.8));
#21093=CARTESIAN_POINT('Origin',(0.,6.,17.3));
#21094=CARTESIAN_POINT('',(0.,0.,0.));
#21095=CARTESIAN_POINT('Origin',(0.05,0.,0.));
#21096=CARTESIAN_POINT('',(0.1,7.34788079488412E-17,0.6));
#21097=CARTESIAN_POINT('Origin',(0.1,0.,0.));
#21098=CARTESIAN_POINT('',(0.,-6.12323399573677E-17,0.5));
#21099=CARTESIAN_POINT('',(0.05,-6.73555739531044E-17,0.55));
#21100=CARTESIAN_POINT('Origin',(0.,0.,0.));
#21101=CARTESIAN_POINT('Origin',(0.,0.,0.));
#21102=CARTESIAN_POINT('',(29.9,-7.34788079488412E-17,0.6));
#21103=CARTESIAN_POINT('Origin',(29.9,0.,0.));
#21104=CARTESIAN_POINT('',(0.,-7.34788079488412E-17,0.6));
#21105=CARTESIAN_POINT('Origin',(0.,0.,0.));
#21106=CARTESIAN_POINT('Origin',(29.95,0.,0.));
#21107=CARTESIAN_POINT('',(30.,6.12323399573677E-17,0.5));
#21108=CARTESIAN_POINT('Origin',(30.,0.,0.));
#21109=CARTESIAN_POINT('',(29.95,-6.73555739531044E-17,0.55));
#21110=CARTESIAN_POINT('Origin',(30.,0.,0.));
#21111=CARTESIAN_POINT('',(0.,0.,0.));
#21112=CARTESIAN_POINT('Origin',(-1.6,0.,1.3));
#21113=CARTESIAN_POINT('',(-1.2,0.340036762718386,1.3));
#21114=CARTESIAN_POINT('',(-1.2,-0.340036762718386,1.3));
#21115=CARTESIAN_POINT('',(-1.2,0.,1.3));
#21116=CARTESIAN_POINT('Origin',(-1.6,0.,1.3));
#21117=CARTESIAN_POINT('Origin',(-1.6,0.,0.6));
#21118=CARTESIAN_POINT('',(-1.2,0.340036762718386,0.6));
#21119=CARTESIAN_POINT('',(-1.2,0.340036762718386,0.6));
#21120=CARTESIAN_POINT('',(-1.2,-0.340036762718386,0.6));
#21121=CARTESIAN_POINT('Origin',(-1.6,0.,0.6));
#21122=CARTESIAN_POINT('',(-1.2,-0.340036762718386,0.6));
#21123=CARTESIAN_POINT('Origin',(1.6,0.,0.6));
#21124=CARTESIAN_POINT('',(1.2,0.340036762718386,1.3));
#21125=CARTESIAN_POINT('',(1.2,0.340036762718386,0.6));
#21126=CARTESIAN_POINT('',(1.2,0.340036762718386,0.6));
#21127=CARTESIAN_POINT('',(1.2,-0.340036762718386,1.3));
#21128=CARTESIAN_POINT('Origin',(1.6,0.,1.3));
#21129=CARTESIAN_POINT('',(1.2,-0.340036762718386,0.6));
#21130=CARTESIAN_POINT('',(1.2,-0.340036762718386,0.6));
#21131=CARTESIAN_POINT('Origin',(1.6,0.,0.6));
#21132=CARTESIAN_POINT('Origin',(1.6,0.,1.3));
#21133=CARTESIAN_POINT('',(1.2,0.,1.3));
#21134=CARTESIAN_POINT('Origin',(-2.1,0.,0.6));
#21135=CARTESIAN_POINT('',(-1.2,0.7,0.6));
#21136=CARTESIAN_POINT('',(-1.2,0.,0.6));
#21137=CARTESIAN_POINT('',(-2.1,0.7,0.6));
#21138=CARTESIAN_POINT('',(-1.2,0.7,0.6));
#21139=CARTESIAN_POINT('',(-2.1,-0.7,0.6));
#21140=CARTESIAN_POINT('',(-2.1,0.,0.6));
#21141=CARTESIAN_POINT('',(-1.2,-0.7,0.6));
#21142=CARTESIAN_POINT('',(-1.2,-0.7,0.6));
#21143=CARTESIAN_POINT('',(-1.2,0.,0.6));
#21144=CARTESIAN_POINT('',(-1.875,3.36777869765522E-17,0.6));
#21145=CARTESIAN_POINT('Origin',(-1.6,0.,0.6));
#21146=CARTESIAN_POINT('Origin',(-1.2,0.,0.6));
#21147=CARTESIAN_POINT('',(-1.2,-0.7,3.75));
#21148=CARTESIAN_POINT('',(-1.2,-0.7,3.75));
#21149=CARTESIAN_POINT('',(-1.2,0.7,3.75));
#21150=CARTESIAN_POINT('',(-1.2,0.,3.75));
#21151=CARTESIAN_POINT('',(-1.2,0.7,3.75));
#21152=CARTESIAN_POINT('',(-1.2,-2.02066721859313E-17,3.515));
#21153=CARTESIAN_POINT('Origin',(-1.2,0.,3.35));
#21154=CARTESIAN_POINT('Origin',(1.2,0.,0.6));
#21155=CARTESIAN_POINT('',(2.1,-0.7,0.6));
#21156=CARTESIAN_POINT('',(2.1,0.7,0.6));
#21157=CARTESIAN_POINT('',(2.1,0.,0.6));
#21158=CARTESIAN_POINT('',(1.2,0.7,0.6));
#21159=CARTESIAN_POINT('',(2.1,0.7,0.6));
#21160=CARTESIAN_POINT('',(1.2,0.,0.6));
#21161=CARTESIAN_POINT('',(1.2,-0.7,0.6));
#21162=CARTESIAN_POINT('',(1.2,0.,0.6));
#21163=CARTESIAN_POINT('',(2.1,-0.7,0.6));
#21164=CARTESIAN_POINT('',(1.325,3.36777869765522E-17,0.6));
#21165=CARTESIAN_POINT('Origin',(1.6,0.,0.6));
#21166=CARTESIAN_POINT('Origin',(0.1,0.,3.35));
#21167=CARTESIAN_POINT('',(0.1,-2.75545529808155E-17,3.575));
#21168=CARTESIAN_POINT('Origin',(0.1,0.,3.35));
#21169=CARTESIAN_POINT('',(1.2,2.75545529808155E-17,3.575));
#21170=CARTESIAN_POINT('',(0.1,-2.75545529808155E-17,3.575));
#21171=CARTESIAN_POINT('Origin',(1.2,0.,3.35));
#21172=CARTESIAN_POINT('Origin',(0.,0.,3.35));
#21173=CARTESIAN_POINT('',(-0.1,2.02066721859313E-17,3.515));
#21174=CARTESIAN_POINT('',(0.,-2.02066721859313E-17,3.515));
#21175=CARTESIAN_POINT('Origin',(-0.1,0.,3.35));
#21176=CARTESIAN_POINT('Origin',(-1.6,0.,-0.05));
#21177=CARTESIAN_POINT('',(-1.875,-3.36777869765522E-17,0.));
#21178=CARTESIAN_POINT('Origin',(-1.6,0.,0.));
#21179=CARTESIAN_POINT('',(-1.875,-3.36777869765522E-17,-0.05));
#21180=CARTESIAN_POINT('Origin',(1.6,0.,-0.05));
#21181=CARTESIAN_POINT('',(1.325,-3.36777869765522E-17,0.));
#21182=CARTESIAN_POINT('Origin',(1.6,0.,0.));
#21183=CARTESIAN_POINT('',(1.325,-3.36777869765522E-17,-0.05));
#21184=CARTESIAN_POINT('Origin',(0.,0.,2.3));
#21185=CARTESIAN_POINT('',(-0.6,-0.7,2.3));
#21186=CARTESIAN_POINT('Origin',(0.,-0.7,2.3));
#21187=CARTESIAN_POINT('',(-0.6,0.7,2.3));
#21188=CARTESIAN_POINT('',(-0.6,0.,2.3));
#21189=CARTESIAN_POINT('Origin',(0.,0.7,2.3));
#21190=CARTESIAN_POINT('Origin',(0.,-0.7,1.875));
#21191=CARTESIAN_POINT('',(-2.1,-0.7,0.));
#21192=CARTESIAN_POINT('',(-2.1,-0.7,0.6));
#21193=CARTESIAN_POINT('',(2.1,-0.7,0.));
#21194=CARTESIAN_POINT('',(-2.1,-0.7,0.));
#21195=CARTESIAN_POINT('',(2.1,-0.7,0.));
#21196=CARTESIAN_POINT('',(1.2,-0.7,3.75));
#21197=CARTESIAN_POINT('',(1.2,-0.7,0.6));
#21198=CARTESIAN_POINT('',(0.1,-0.7,3.75));
#21199=CARTESIAN_POINT('',(1.2,-0.7,3.75));
#21200=CARTESIAN_POINT('',(0.1,-0.7,2.95));
#21201=CARTESIAN_POINT('',(0.1,-0.7,3.75));
#21202=CARTESIAN_POINT('',(-0.1,-0.7,2.95));
#21203=CARTESIAN_POINT('',(0.1,-0.7,2.95));
#21204=CARTESIAN_POINT('',(-0.1,-0.7,3.75));
#21205=CARTESIAN_POINT('',(-0.1,-0.7,2.95));
#21206=CARTESIAN_POINT('',(-0.1,-0.7,3.75));
#21207=CARTESIAN_POINT('Origin',(-2.1,0.,0.));
#21208=CARTESIAN_POINT('',(-2.1,0.7,0.));
#21209=CARTESIAN_POINT('',(-2.1,0.7,0.6));
#21210=CARTESIAN_POINT('',(-2.1,0.,0.));
#21211=CARTESIAN_POINT('Origin',(2.1,0.,0.));
#21212=CARTESIAN_POINT('',(2.1,0.7,0.));
#21213=CARTESIAN_POINT('',(-2.1,0.7,0.));
#21214=CARTESIAN_POINT('',(2.1,0.,0.));
#21215=CARTESIAN_POINT('Origin',(2.1,0.,0.6));
#21216=CARTESIAN_POINT('',(2.1,0.7,0.));
#21217=CARTESIAN_POINT('Origin',(1.2,0.,3.75));
#21218=CARTESIAN_POINT('',(1.2,0.7,3.75));
#21219=CARTESIAN_POINT('',(1.2,0.7,0.6));
#21220=CARTESIAN_POINT('',(1.2,0.,3.75));
#21221=CARTESIAN_POINT('Origin',(0.1,0.,3.75));
#21222=CARTESIAN_POINT('',(0.1,0.7,3.75));
#21223=CARTESIAN_POINT('',(1.2,0.7,3.75));
#21224=CARTESIAN_POINT('',(0.1,0.,3.75));
#21225=CARTESIAN_POINT('Origin',(0.1,0.,2.95));
#21226=CARTESIAN_POINT('',(0.1,0.7,2.95));
#21227=CARTESIAN_POINT('',(0.1,0.7,3.75));
#21228=CARTESIAN_POINT('',(0.1,0.,2.95));
#21229=CARTESIAN_POINT('Origin',(-0.1,0.,2.95));
#21230=CARTESIAN_POINT('',(-0.1,0.7,2.95));
#21231=CARTESIAN_POINT('',(0.1,0.7,2.95));
#21232=CARTESIAN_POINT('',(-0.1,0.,2.95));
#21233=CARTESIAN_POINT('Origin',(-0.1,0.,3.75));
#21234=CARTESIAN_POINT('',(-0.1,0.7,3.75));
#21235=CARTESIAN_POINT('',(-0.1,0.7,2.95));
#21236=CARTESIAN_POINT('',(-0.1,0.,3.75));
#21237=CARTESIAN_POINT('Origin',(-1.2,0.,3.75));
#21238=CARTESIAN_POINT('',(-0.1,0.7,3.75));
#21239=CARTESIAN_POINT('Origin',(0.,0.7,1.875));
#21240=CARTESIAN_POINT('',(0.,0.,0.));
#21241=CARTESIAN_POINT('Origin',(0.115470053837925,-0.5,-0.2));
#21242=CARTESIAN_POINT('',(0.23094010767585,-0.5,0.));
#21243=CARTESIAN_POINT('',(0.115470053837925,-0.5,-0.2));
#21244=CARTESIAN_POINT('',(0.23094010767585,-0.5,0.));
#21245=CARTESIAN_POINT('',(0.115470053837925,-0.8,-0.2));
#21246=CARTESIAN_POINT('',(0.115470053837925,-0.5,-0.2));
#21247=CARTESIAN_POINT('',(0.23094010767585,-0.8,0.));
#21248=CARTESIAN_POINT('',(0.23094010767585,-0.8,0.));
#21249=CARTESIAN_POINT('',(0.23094010767585,-0.5,0.));
#21250=CARTESIAN_POINT('Origin',(-0.115470053837925,-0.5,-0.2));
#21251=CARTESIAN_POINT('',(-0.115470053837925,-0.5,-0.2));
#21252=CARTESIAN_POINT('',(0.115470053837925,-0.5,-0.2));
#21253=CARTESIAN_POINT('',(-0.115470053837925,-0.8,-0.2));
#21254=CARTESIAN_POINT('',(-0.115470053837925,-0.5,-0.2));
#21255=CARTESIAN_POINT('',(0.115470053837925,-0.8,-0.2));
#21256=CARTESIAN_POINT('Origin',(-0.23094010767585,-0.5,-2.77555756156289E-17));
#21257=CARTESIAN_POINT('',(-0.23094010767585,-0.5,-2.82820063659975E-17));
#21258=CARTESIAN_POINT('',(-0.115470053837925,-0.5,-0.2));
#21259=CARTESIAN_POINT('',(-0.23094010767585,-0.8,-2.77555756156289E-17));
#21260=CARTESIAN_POINT('',(-0.23094010767585,-0.5,-2.82820063659975E-17));
#21261=CARTESIAN_POINT('',(-0.115470053837925,-0.8,-0.2));
#21262=CARTESIAN_POINT('Origin',(-0.115470053837925,-0.5,0.2));
#21263=CARTESIAN_POINT('',(-0.115470053837925,-0.5,0.2));
#21264=CARTESIAN_POINT('',(-0.23094010767585,-0.5,-2.82820063659975E-17));
#21265=CARTESIAN_POINT('',(-0.115470053837925,-0.8,0.2));
#21266=CARTESIAN_POINT('',(-0.115470053837925,-0.5,0.2));
#21267=CARTESIAN_POINT('',(-0.23094010767585,-0.8,-2.82820063659975E-17));
#21268=CARTESIAN_POINT('Origin',(0.115470053837925,-0.5,0.2));
#21269=CARTESIAN_POINT('',(0.115470053837925,-0.5,0.2));
#21270=CARTESIAN_POINT('',(-0.115470053837925,-0.5,0.2));
#21271=CARTESIAN_POINT('',(0.115470053837925,-0.8,0.2));
#21272=CARTESIAN_POINT('',(0.115470053837925,-0.5,0.2));
#21273=CARTESIAN_POINT('',(-0.115470053837925,-0.8,0.2));
#21274=CARTESIAN_POINT('Origin',(0.23094010767585,-0.5,0.));
#21275=CARTESIAN_POINT('',(0.115470053837925,-0.5,0.2));
#21276=CARTESIAN_POINT('',(0.115470053837925,-0.8,0.2));
#21277=CARTESIAN_POINT('Origin',(0.,-0.5,0.));
#21278=CARTESIAN_POINT('Origin',(0.,-0.8,0.));
#21279=CARTESIAN_POINT('Origin',(0.,-1.4,0.));
#21280=CARTESIAN_POINT('',(-0.24505,-1.4,3.00099698131059E-17));
#21281=CARTESIAN_POINT('Origin',(0.,-1.4,0.));
#21282=CARTESIAN_POINT('Origin',(0.375,0.5,0.));
#21283=CARTESIAN_POINT('',(-0.375,0.5,-4.59242549680257E-17));
#21284=CARTESIAN_POINT('Origin',(0.,0.5,0.));
#21285=CARTESIAN_POINT('Origin',(0.,0.475,0.));
#21286=CARTESIAN_POINT('',(-0.425,0.45,-5.20474889637625E-17));
#21287=CARTESIAN_POINT('Origin',(0.,0.45,0.));
#21288=CARTESIAN_POINT('',(-0.4,0.475,-4.89858719658941E-17));
#21289=CARTESIAN_POINT('Origin',(0.,0.24,0.));
#21290=CARTESIAN_POINT('',(-0.425,0.0299999999999998,-5.20474889637625E-17));
#21291=CARTESIAN_POINT('Origin',(0.,0.0299999999999998,0.));
#21292=CARTESIAN_POINT('',(-0.425,0.24,-5.20474889637625E-17));
#21293=CARTESIAN_POINT('Origin',(0.,0.0150000000000001,0.));
#21294=CARTESIAN_POINT('',(-0.395,4.85722573273506E-17,-4.83735485663204E-17));
#21295=CARTESIAN_POINT('Origin',(0.,0.,0.));
#21296=CARTESIAN_POINT('',(-0.41,0.0150000000000001,-5.02105187650415E-17));
#21297=CARTESIAN_POINT('Origin',(0.27,0.,0.));
#21298=CARTESIAN_POINT('',(-0.27,0.,-3.30654635769785E-17));
#21299=CARTESIAN_POINT('Origin',(0.,0.,0.));
#21300=CARTESIAN_POINT('Origin',(0.,-0.02,0.));
#21301=CARTESIAN_POINT('',(-0.24505,-0.0498999999999999,3.00099698131059E-17));
#21302=CARTESIAN_POINT('Origin',(0.,-0.0498999999999999,0.));
#21303=CARTESIAN_POINT('',(-0.26,-0.02,-3.18408167778312E-17));
#21304=CARTESIAN_POINT('Origin',(0.,-0.995,0.));
#21305=CARTESIAN_POINT('',(-0.24505,-0.995,-3.00099698131059E-17));
#21306=CARTESIAN_POINT('',(0.,0.,0.));
#21307=CARTESIAN_POINT('Origin',(0.375,0.5,0.));
#21308=CARTESIAN_POINT('',(-0.375,0.5,-4.59242549680257E-17));
#21309=CARTESIAN_POINT('Origin',(0.,0.5,0.));
#21310=CARTESIAN_POINT('Origin',(0.,0.475,0.));
#21311=CARTESIAN_POINT('',(-0.425,0.45,-5.20474889637625E-17));
#21312=CARTESIAN_POINT('Origin',(0.,0.45,0.));
#21313=CARTESIAN_POINT('',(-0.4,0.475,-4.89858719658941E-17));
#21314=CARTESIAN_POINT('Origin',(0.,0.24,0.));
#21315=CARTESIAN_POINT('',(-0.425,0.0299999999999998,-5.20474889637625E-17));
#21316=CARTESIAN_POINT('Origin',(0.,0.0299999999999998,0.));
#21317=CARTESIAN_POINT('',(-0.425,0.24,-5.20474889637625E-17));
#21318=CARTESIAN_POINT('Origin',(0.,0.0150000000000001,0.));
#21319=CARTESIAN_POINT('',(-0.395,4.85722573273506E-17,-4.83735485663204E-17));
#21320=CARTESIAN_POINT('Origin',(0.,0.,0.));
#21321=CARTESIAN_POINT('',(-0.41,0.0150000000000001,-5.02105187650415E-17));
#21322=CARTESIAN_POINT('Origin',(0.27,0.,0.));
#21323=CARTESIAN_POINT('',(-0.27,0.,-3.30654635769785E-17));
#21324=CARTESIAN_POINT('Origin',(0.,0.,0.));
#21325=CARTESIAN_POINT('Origin',(0.,-0.02,0.));
#21326=CARTESIAN_POINT('',(-0.24505,-0.0498999999999999,3.00099698131059E-17));
#21327=CARTESIAN_POINT('Origin',(0.,-0.0498999999999999,0.));
#21328=CARTESIAN_POINT('',(-0.26,-0.02,-3.18408167778312E-17));
#21329=CARTESIAN_POINT('Origin',(0.,-0.995,0.));
#21330=CARTESIAN_POINT('',(-0.24505,-1.95495,3.00099698131059E-17));
#21331=CARTESIAN_POINT('Origin',(0.,-1.95495,0.));
#21332=CARTESIAN_POINT('',(-0.24505,-0.995,-3.00099698131059E-17));
#21333=CARTESIAN_POINT('Origin',(0.,-1.975,0.));
#21334=CARTESIAN_POINT('',(-0.2,-2.,-2.44929359829471E-17));
#21335=CARTESIAN_POINT('Origin',(0.,-2.,0.));
#21336=CARTESIAN_POINT('',(-0.225,-1.975,-2.75545529808154E-17));
#21337=CARTESIAN_POINT('Origin',(0.,-2.,0.));
#21338=CARTESIAN_POINT('Origin',(0.115470053837925,-0.5,-0.2));
#21339=CARTESIAN_POINT('',(0.23094010767585,-0.5,0.));
#21340=CARTESIAN_POINT('',(0.115470053837925,-0.5,-0.2));
#21341=CARTESIAN_POINT('',(0.23094010767585,-0.5,0.));
#21342=CARTESIAN_POINT('',(0.115470053837925,-0.8,-0.2));
#21343=CARTESIAN_POINT('',(0.115470053837925,-0.5,-0.2));
#21344=CARTESIAN_POINT('',(0.23094010767585,-0.8,0.));
#21345=CARTESIAN_POINT('',(0.23094010767585,-0.8,0.));
#21346=CARTESIAN_POINT('',(0.23094010767585,-0.5,0.));
#21347=CARTESIAN_POINT('Origin',(-0.115470053837925,-0.5,-0.2));
#21348=CARTESIAN_POINT('',(-0.115470053837925,-0.5,-0.2));
#21349=CARTESIAN_POINT('',(0.115470053837925,-0.5,-0.2));
#21350=CARTESIAN_POINT('',(-0.115470053837925,-0.8,-0.2));
#21351=CARTESIAN_POINT('',(-0.115470053837925,-0.5,-0.2));
#21352=CARTESIAN_POINT('',(0.115470053837925,-0.8,-0.2));
#21353=CARTESIAN_POINT('Origin',(-0.23094010767585,-0.5,-2.77555756156289E-17));
#21354=CARTESIAN_POINT('',(-0.23094010767585,-0.5,-2.82820063659975E-17));
#21355=CARTESIAN_POINT('',(-0.115470053837925,-0.5,-0.2));
#21356=CARTESIAN_POINT('',(-0.23094010767585,-0.8,-2.77555756156289E-17));
#21357=CARTESIAN_POINT('',(-0.23094010767585,-0.5,-2.82820063659975E-17));
#21358=CARTESIAN_POINT('',(-0.115470053837925,-0.8,-0.2));
#21359=CARTESIAN_POINT('Origin',(-0.115470053837925,-0.5,0.2));
#21360=CARTESIAN_POINT('',(-0.115470053837925,-0.5,0.2));
#21361=CARTESIAN_POINT('',(-0.23094010767585,-0.5,-2.82820063659975E-17));
#21362=CARTESIAN_POINT('',(-0.115470053837925,-0.8,0.2));
#21363=CARTESIAN_POINT('',(-0.115470053837925,-0.5,0.2));
#21364=CARTESIAN_POINT('',(-0.23094010767585,-0.8,-2.82820063659975E-17));
#21365=CARTESIAN_POINT('Origin',(0.115470053837925,-0.5,0.2));
#21366=CARTESIAN_POINT('',(0.115470053837925,-0.5,0.2));
#21367=CARTESIAN_POINT('',(-0.115470053837925,-0.5,0.2));
#21368=CARTESIAN_POINT('',(0.115470053837925,-0.8,0.2));
#21369=CARTESIAN_POINT('',(0.115470053837925,-0.5,0.2));
#21370=CARTESIAN_POINT('',(-0.115470053837925,-0.8,0.2));
#21371=CARTESIAN_POINT('Origin',(0.23094010767585,-0.5,0.));
#21372=CARTESIAN_POINT('',(0.115470053837925,-0.5,0.2));
#21373=CARTESIAN_POINT('',(0.115470053837925,-0.8,0.2));
#21374=CARTESIAN_POINT('Origin',(0.,-0.5,0.));
#21375=CARTESIAN_POINT('Origin',(0.,-0.8,0.));
#21376=CARTESIAN_POINT('',(0.,0.,0.));
#21377=CARTESIAN_POINT('',(0.,0.,0.));
#21378=CARTESIAN_POINT('Origin',(0.,-1.,15.));
#21379=CARTESIAN_POINT('',(-0.225,-1.,15.1));
#21380=CARTESIAN_POINT('Origin',(0.,-1.,15.1));
#21381=CARTESIAN_POINT('',(-0.225,-1.,16.3));
#21382=CARTESIAN_POINT('',(-0.225,-1.,15.));
#21383=CARTESIAN_POINT('Origin',(0.,-1.,16.3));
#21384=CARTESIAN_POINT('Origin',(1.,0.,15.));
#21385=CARTESIAN_POINT('',(0.775,-2.75545529808155E-17,15.1));
#21386=CARTESIAN_POINT('Origin',(1.,0.,15.1));
#21387=CARTESIAN_POINT('',(0.775,2.75545529808155E-17,16.3));
#21388=CARTESIAN_POINT('',(0.775,-2.75545529808155E-17,15.));
#21389=CARTESIAN_POINT('Origin',(1.,0.,16.3));
#21390=CARTESIAN_POINT('Origin',(-1.,0.,15.));
#21391=CARTESIAN_POINT('',(-1.225,-2.75545529808154E-17,15.1));
#21392=CARTESIAN_POINT('Origin',(-1.,0.,15.1));
#21393=CARTESIAN_POINT('',(-1.225,2.75545529808154E-17,16.3));
#21394=CARTESIAN_POINT('',(-1.225,-2.75545529808154E-17,15.));
#21395=CARTESIAN_POINT('Origin',(-1.,0.,16.3));
#21396=CARTESIAN_POINT('Origin',(0.,1.,15.));
#21397=CARTESIAN_POINT('',(-0.225,1.,15.1));
#21398=CARTESIAN_POINT('Origin',(0.,1.,15.1));
#21399=CARTESIAN_POINT('',(-0.225,1.,16.3));
#21400=CARTESIAN_POINT('',(-0.225,1.,15.));
#21401=CARTESIAN_POINT('Origin',(0.,1.,16.3));
#21402=CARTESIAN_POINT('Origin',(4.86862915010152,2.86862915010152,15.));
#21403=CARTESIAN_POINT('',(4.64362915010152,2.86862915010152,15.1));
#21404=CARTESIAN_POINT('Origin',(4.86862915010152,2.86862915010152,15.1));
#21405=CARTESIAN_POINT('',(4.64362915010152,2.86862915010152,16.3));
#21406=CARTESIAN_POINT('',(4.64362915010152,2.86862915010152,15.));
#21407=CARTESIAN_POINT('Origin',(4.86862915010152,2.86862915010152,16.3));
#21408=CARTESIAN_POINT('Origin',(4.86862915010152,5.13137084989848,15.));
#21409=CARTESIAN_POINT('',(4.64362915010152,5.13137084989848,15.1));
#21410=CARTESIAN_POINT('Origin',(4.86862915010152,5.13137084989848,15.1));
#21411=CARTESIAN_POINT('',(4.64362915010152,5.13137084989848,16.3));
#21412=CARTESIAN_POINT('',(4.64362915010152,5.13137084989848,15.));
#21413=CARTESIAN_POINT('Origin',(4.86862915010152,5.13137084989848,16.3));
#21414=CARTESIAN_POINT('Origin',(7.13137084989848,5.13137084989848,15.));
#21415=CARTESIAN_POINT('',(6.90637084989848,5.13137084989848,15.1));
#21416=CARTESIAN_POINT('Origin',(7.13137084989848,5.13137084989848,15.1));
#21417=CARTESIAN_POINT('',(6.90637084989848,5.13137084989848,16.3));
#21418=CARTESIAN_POINT('',(6.90637084989848,5.13137084989848,15.));
#21419=CARTESIAN_POINT('Origin',(7.13137084989848,5.13137084989848,16.3));
#21420=CARTESIAN_POINT('Origin',(7.13137084989848,2.86862915010152,15.));
#21421=CARTESIAN_POINT('',(6.90637084989848,2.86862915010152,15.1));
#21422=CARTESIAN_POINT('Origin',(7.13137084989848,2.86862915010152,15.1));
#21423=CARTESIAN_POINT('',(6.90637084989848,2.86862915010152,16.3));
#21424=CARTESIAN_POINT('',(6.90637084989848,2.86862915010152,15.));
#21425=CARTESIAN_POINT('Origin',(7.13137084989848,2.86862915010152,16.3));
#21426=CARTESIAN_POINT('Origin',(4.86862915010152,-5.13137084989848,15.));
#21427=CARTESIAN_POINT('',(4.64362915010152,-5.13137084989848,15.1));
#21428=CARTESIAN_POINT('Origin',(4.86862915010152,-5.13137084989848,15.1));
#21429=CARTESIAN_POINT('',(4.64362915010152,-5.13137084989848,16.3));
#21430=CARTESIAN_POINT('',(4.64362915010152,-5.13137084989848,15.));
#21431=CARTESIAN_POINT('Origin',(4.86862915010152,-5.13137084989848,16.3));
#21432=CARTESIAN_POINT('Origin',(4.86862915010152,-2.86862915010152,15.));
#21433=CARTESIAN_POINT('',(4.64362915010152,-2.86862915010152,15.1));
#21434=CARTESIAN_POINT('Origin',(4.86862915010152,-2.86862915010152,15.1));
#21435=CARTESIAN_POINT('',(4.64362915010152,-2.86862915010152,16.3));
#21436=CARTESIAN_POINT('',(4.64362915010152,-2.86862915010152,15.));
#21437=CARTESIAN_POINT('Origin',(4.86862915010152,-2.86862915010152,16.3));
#21438=CARTESIAN_POINT('Origin',(7.13137084989848,-2.86862915010152,15.));
#21439=CARTESIAN_POINT('',(6.90637084989848,-2.86862915010152,15.1));
#21440=CARTESIAN_POINT('Origin',(7.13137084989848,-2.86862915010152,15.1));
#21441=CARTESIAN_POINT('',(6.90637084989848,-2.86862915010152,16.3));
#21442=CARTESIAN_POINT('',(6.90637084989848,-2.86862915010152,15.));
#21443=CARTESIAN_POINT('Origin',(7.13137084989848,-2.86862915010152,16.3));
#21444=CARTESIAN_POINT('Origin',(7.13137084989848,-5.13137084989848,15.));
#21445=CARTESIAN_POINT('',(6.90637084989848,-5.13137084989848,15.1));
#21446=CARTESIAN_POINT('Origin',(7.13137084989848,-5.13137084989848,15.1));
#21447=CARTESIAN_POINT('',(6.90637084989848,-5.13137084989848,16.3));
#21448=CARTESIAN_POINT('',(6.90637084989848,-5.13137084989848,15.));
#21449=CARTESIAN_POINT('Origin',(7.13137084989848,-5.13137084989848,16.3));
#21450=CARTESIAN_POINT('Origin',(-7.13137084989848,2.86862915010152,15.));
#21451=CARTESIAN_POINT('',(-7.35637084989848,2.86862915010152,15.1));
#21452=CARTESIAN_POINT('Origin',(-7.13137084989848,2.86862915010152,15.1));
#21453=CARTESIAN_POINT('',(-7.35637084989848,2.86862915010152,16.3));
#21454=CARTESIAN_POINT('',(-7.35637084989848,2.86862915010152,15.));
#21455=CARTESIAN_POINT('Origin',(-7.13137084989848,2.86862915010152,16.3));
#21456=CARTESIAN_POINT('Origin',(-7.13137084989848,5.13137084989848,15.));
#21457=CARTESIAN_POINT('',(-7.35637084989848,5.13137084989848,15.1));
#21458=CARTESIAN_POINT('Origin',(-7.13137084989848,5.13137084989848,15.1));
#21459=CARTESIAN_POINT('',(-7.35637084989848,5.13137084989848,16.3));
#21460=CARTESIAN_POINT('',(-7.35637084989848,5.13137084989848,15.));
#21461=CARTESIAN_POINT('Origin',(-7.13137084989848,5.13137084989848,16.3));
#21462=CARTESIAN_POINT('Origin',(-4.86862915010152,5.13137084989848,15.));
#21463=CARTESIAN_POINT('',(-5.09362915010152,5.13137084989848,15.1));
#21464=CARTESIAN_POINT('Origin',(-4.86862915010152,5.13137084989848,15.1));
#21465=CARTESIAN_POINT('',(-5.09362915010152,5.13137084989848,16.3));
#21466=CARTESIAN_POINT('',(-5.09362915010152,5.13137084989848,15.));
#21467=CARTESIAN_POINT('Origin',(-4.86862915010152,5.13137084989848,16.3));
#21468=CARTESIAN_POINT('Origin',(-4.86862915010152,2.86862915010152,15.));
#21469=CARTESIAN_POINT('',(-5.09362915010152,2.86862915010152,15.1));
#21470=CARTESIAN_POINT('Origin',(-4.86862915010152,2.86862915010152,15.1));
#21471=CARTESIAN_POINT('',(-5.09362915010152,2.86862915010152,16.3));
#21472=CARTESIAN_POINT('',(-5.09362915010152,2.86862915010152,15.));
#21473=CARTESIAN_POINT('Origin',(-4.86862915010152,2.86862915010152,16.3));
#21474=CARTESIAN_POINT('Origin',(-7.13137084989848,-5.13137084989848,15.));
#21475=CARTESIAN_POINT('',(-7.35637084989848,-5.13137084989848,15.1));
#21476=CARTESIAN_POINT('Origin',(-7.13137084989848,-5.13137084989848,15.1));
#21477=CARTESIAN_POINT('',(-7.35637084989848,-5.13137084989848,16.3));
#21478=CARTESIAN_POINT('',(-7.35637084989848,-5.13137084989848,15.));
#21479=CARTESIAN_POINT('Origin',(-7.13137084989848,-5.13137084989848,16.3));
#21480=CARTESIAN_POINT('Origin',(-7.13137084989848,-2.86862915010152,15.));
#21481=CARTESIAN_POINT('',(-7.35637084989848,-2.86862915010152,15.1));
#21482=CARTESIAN_POINT('Origin',(-7.13137084989848,-2.86862915010152,15.1));
#21483=CARTESIAN_POINT('',(-7.35637084989848,-2.86862915010152,16.3));
#21484=CARTESIAN_POINT('',(-7.35637084989848,-2.86862915010152,15.));
#21485=CARTESIAN_POINT('Origin',(-7.13137084989848,-2.86862915010152,16.3));
#21486=CARTESIAN_POINT('Origin',(-4.86862915010152,-2.86862915010152,15.));
#21487=CARTESIAN_POINT('',(-5.09362915010152,-2.86862915010152,15.1));
#21488=CARTESIAN_POINT('Origin',(-4.86862915010152,-2.86862915010152,15.1));
#21489=CARTESIAN_POINT('',(-5.09362915010152,-2.86862915010152,16.3));
#21490=CARTESIAN_POINT('',(-5.09362915010152,-2.86862915010152,15.));
#21491=CARTESIAN_POINT('Origin',(-4.86862915010152,-2.86862915010152,16.3));
#21492=CARTESIAN_POINT('Origin',(-4.86862915010152,-5.13137084989848,15.));
#21493=CARTESIAN_POINT('',(-5.09362915010152,-5.13137084989848,15.1));
#21494=CARTESIAN_POINT('Origin',(-4.86862915010152,-5.13137084989848,15.1));
#21495=CARTESIAN_POINT('',(-5.09362915010152,-5.13137084989848,16.3));
#21496=CARTESIAN_POINT('',(-5.09362915010152,-5.13137084989848,15.));
#21497=CARTESIAN_POINT('Origin',(-4.86862915010152,-5.13137084989848,16.3));
#21498=CARTESIAN_POINT('Origin',(6.,-4.,15.));
#21499=CARTESIAN_POINT('',(5.375,-4.,15.1));
#21500=CARTESIAN_POINT('Origin',(6.,-4.,15.1));
#21501=CARTESIAN_POINT('',(5.375,-4.,16.3));
#21502=CARTESIAN_POINT('',(5.375,-4.,15.));
#21503=CARTESIAN_POINT('Origin',(6.,-4.,16.3));
#21504=CARTESIAN_POINT('Origin',(-6.,4.,15.));
#21505=CARTESIAN_POINT('',(-6.625,4.,15.1));
#21506=CARTESIAN_POINT('Origin',(-6.,4.,15.1));
#21507=CARTESIAN_POINT('',(-6.625,4.,16.3));
#21508=CARTESIAN_POINT('',(-6.625,4.,15.));
#21509=CARTESIAN_POINT('Origin',(-6.,4.,16.3));
#21510=CARTESIAN_POINT('Origin',(-6.,-4.,15.));
#21511=CARTESIAN_POINT('',(-6.625,-4.,15.1));
#21512=CARTESIAN_POINT('Origin',(-6.,-4.,15.1));
#21513=CARTESIAN_POINT('',(-6.625,-4.,16.3));
#21514=CARTESIAN_POINT('',(-6.625,-4.,15.));
#21515=CARTESIAN_POINT('Origin',(-6.,-4.,16.3));
#21516=CARTESIAN_POINT('Origin',(6.,4.,15.));
#21517=CARTESIAN_POINT('',(5.375,4.,15.1));
#21518=CARTESIAN_POINT('Origin',(6.,4.,15.1));
#21519=CARTESIAN_POINT('',(5.375,4.,16.3));
#21520=CARTESIAN_POINT('',(5.375,4.,15.));
#21521=CARTESIAN_POINT('Origin',(6.,4.,16.3));
#21522=CARTESIAN_POINT('Origin',(8.5,6.5,15.1));
#21523=CARTESIAN_POINT('',(8.5,6.5,15.1));
#21524=CARTESIAN_POINT('',(-8.5,6.5,15.1));
#21525=CARTESIAN_POINT('',(8.5,6.5,15.1));
#21526=CARTESIAN_POINT('',(-8.5,6.5,16.3));
#21527=CARTESIAN_POINT('',(-8.5,6.5,15.1));
#21528=CARTESIAN_POINT('',(8.5,6.5,16.3));
#21529=CARTESIAN_POINT('',(8.5,6.5,16.3));
#21530=CARTESIAN_POINT('',(8.5,6.5,15.1));
#21531=CARTESIAN_POINT('Origin',(8.5,-6.5,15.1));
#21532=CARTESIAN_POINT('',(8.5,-6.5,15.1));
#21533=CARTESIAN_POINT('',(8.5,-6.5,15.1));
#21534=CARTESIAN_POINT('',(8.5,-6.5,16.3));
#21535=CARTESIAN_POINT('',(8.5,-6.5,16.3));
#21536=CARTESIAN_POINT('',(8.5,-6.5,15.1));
#21537=CARTESIAN_POINT('Origin',(-8.5,-6.5,15.1));
#21538=CARTESIAN_POINT('',(-8.5,-6.5,15.1));
#21539=CARTESIAN_POINT('',(-8.5,-6.5,15.1));
#21540=CARTESIAN_POINT('',(-8.5,-6.5,16.3));
#21541=CARTESIAN_POINT('',(-8.5,-6.5,16.3));
#21542=CARTESIAN_POINT('',(-8.5,-6.5,15.1));
#21543=CARTESIAN_POINT('Origin',(-8.5,6.5,15.1));
#21544=CARTESIAN_POINT('',(-8.5,6.5,15.1));
#21545=CARTESIAN_POINT('',(-8.5,6.5,16.3));
#21546=CARTESIAN_POINT('Origin',(0.,0.,16.3));
#21547=CARTESIAN_POINT('Origin',(0.,0.,15.1));
#21548=CARTESIAN_POINT('',(0.,0.,0.));
#21549=CARTESIAN_POINT('Origin',(-7.13137084989848,-5.13137084989848,14.));
#21550=CARTESIAN_POINT('',(-6.96707794165985,-5.14662995545858,14.));
#21551=CARTESIAN_POINT('',(-7.14662995545858,-4.96707794165985,14.));
#21552=CARTESIAN_POINT('Origin',(-6.,-4.,14.));
#21553=CARTESIAN_POINT('Origin',(-7.13137084989848,-5.13137084989848,14.));
#21554=CARTESIAN_POINT('Origin',(-7.13137084989848,-5.13137084989848,14.));
#21555=CARTESIAN_POINT('',(-6.96707794165985,-5.14662995545858,14.6));
#21556=CARTESIAN_POINT('',(-6.96707794165985,-5.14662995545858,14.));
#21557=CARTESIAN_POINT('',(-7.29637084989848,-5.13137084989848,14.6));
#21558=CARTESIAN_POINT('Origin',(-7.13137084989848,-5.13137084989848,14.6));
#21559=CARTESIAN_POINT('',(-7.29637084989848,-5.13137084989848,15.1));
#21560=CARTESIAN_POINT('',(-7.29637084989848,-5.13137084989848,14.));
#21561=CARTESIAN_POINT('Origin',(-7.13137084989848,-5.13137084989848,15.1));
#21562=CARTESIAN_POINT('',(-7.14662995545858,-4.96707794165985,14.6));
#21563=CARTESIAN_POINT('Origin',(-7.13137084989848,-5.13137084989848,14.6));
#21564=CARTESIAN_POINT('',(-7.14662995545858,-4.96707794165985,14.));
#21565=CARTESIAN_POINT('Origin',(-7.13137084989848,-2.86862915010152,14.));
#21566=CARTESIAN_POINT('',(-7.14662995545858,-3.03292205834015,14.));
#21567=CARTESIAN_POINT('',(-6.96707794165985,-2.85337004454142,14.));
#21568=CARTESIAN_POINT('Origin',(-6.,-4.,14.));
#21569=CARTESIAN_POINT('Origin',(-7.13137084989848,-2.86862915010152,14.));
#21570=CARTESIAN_POINT('Origin',(-7.13137084989848,-2.86862915010152,14.));
#21571=CARTESIAN_POINT('',(-7.14662995545858,-3.03292205834015,14.6));
#21572=CARTESIAN_POINT('',(-7.14662995545858,-3.03292205834015,14.));
#21573=CARTESIAN_POINT('',(-7.29637084989848,-2.86862915010152,14.6));
#21574=CARTESIAN_POINT('Origin',(-7.13137084989848,-2.86862915010152,14.6));
#21575=CARTESIAN_POINT('',(-7.29637084989848,-2.86862915010152,15.1));
#21576=CARTESIAN_POINT('',(-7.29637084989848,-2.86862915010152,14.));
#21577=CARTESIAN_POINT('Origin',(-7.13137084989848,-2.86862915010152,15.1));
#21578=CARTESIAN_POINT('',(-6.96707794165985,-2.85337004454142,14.6));
#21579=CARTESIAN_POINT('Origin',(-7.13137084989848,-2.86862915010152,14.6));
#21580=CARTESIAN_POINT('',(-6.96707794165985,-2.85337004454142,14.));
#21581=CARTESIAN_POINT('Origin',(-4.86862915010152,-2.86862915010152,14.));
#21582=CARTESIAN_POINT('',(-5.03292205834015,-2.85337004454142,14.));
#21583=CARTESIAN_POINT('',(-4.85337004454142,-3.03292205834015,14.));
#21584=CARTESIAN_POINT('Origin',(-6.,-4.,14.));
#21585=CARTESIAN_POINT('',(-5.03362915010152,-2.86862915010152,14.));
#21586=CARTESIAN_POINT('Origin',(-4.86862915010152,-2.86862915010152,14.));
#21587=CARTESIAN_POINT('Origin',(-4.86862915010152,-2.86862915010152,14.));
#21588=CARTESIAN_POINT('Origin',(-4.86862915010152,-2.86862915010152,14.));
#21589=CARTESIAN_POINT('',(-5.03292205834015,-2.85337004454142,14.6));
#21590=CARTESIAN_POINT('',(-5.03292205834015,-2.85337004454142,14.));
#21591=CARTESIAN_POINT('',(-4.85337004454142,-3.03292205834015,14.6));
#21592=CARTESIAN_POINT('Origin',(-4.86862915010152,-2.86862915010152,14.6));
#21593=CARTESIAN_POINT('',(-4.85337004454142,-3.03292205834015,14.));
#21594=CARTESIAN_POINT('',(-5.03362915010152,-2.86862915010152,15.1));
#21595=CARTESIAN_POINT('',(-5.03362915010152,-2.86862915010152,14.));
#21596=CARTESIAN_POINT('Origin',(-4.86862915010152,-2.86862915010152,15.1));
#21597=CARTESIAN_POINT('Origin',(-4.86862915010152,-5.13137084989848,14.));
#21598=CARTESIAN_POINT('',(-4.85337004454142,-4.96707794165985,14.));
#21599=CARTESIAN_POINT('',(-5.03292205834015,-5.14662995545858,14.));
#21600=CARTESIAN_POINT('Origin',(-6.,-4.,14.));
#21601=CARTESIAN_POINT('',(-5.03362915010152,-5.13137084989848,14.));
#21602=CARTESIAN_POINT('Origin',(-4.86862915010152,-5.13137084989848,14.));
#21603=CARTESIAN_POINT('Origin',(-4.86862915010152,-5.13137084989848,14.));
#21604=CARTESIAN_POINT('Origin',(-4.86862915010152,-5.13137084989848,14.));
#21605=CARTESIAN_POINT('',(-4.85337004454142,-4.96707794165985,14.6));
#21606=CARTESIAN_POINT('',(-4.85337004454142,-4.96707794165985,14.));
#21607=CARTESIAN_POINT('',(-5.03292205834015,-5.14662995545858,14.6));
#21608=CARTESIAN_POINT('Origin',(-4.86862915010152,-5.13137084989848,14.6));
#21609=CARTESIAN_POINT('',(-5.03292205834015,-5.14662995545858,14.));
#21610=CARTESIAN_POINT('',(-5.03362915010152,-5.13137084989848,15.1));
#21611=CARTESIAN_POINT('',(-5.03362915010152,-5.13137084989848,14.));
#21612=CARTESIAN_POINT('Origin',(-4.86862915010152,-5.13137084989848,15.1));
#21613=CARTESIAN_POINT('Origin',(-6.,-4.,11.5));
#21614=CARTESIAN_POINT('',(-7.5,-4.,14.6));
#21615=CARTESIAN_POINT('Origin',(-6.,-4.,14.6));
#21616=CARTESIAN_POINT('',(-7.5,-4.,11.5));
#21617=CARTESIAN_POINT('',(-7.5,-4.,11.5));
#21618=CARTESIAN_POINT('Origin',(-6.,-4.,11.5));
#21619=CARTESIAN_POINT('Origin',(-6.,-4.,14.6));
#21620=CARTESIAN_POINT('Origin',(-6.,-4.,14.6));
#21621=CARTESIAN_POINT('Origin',(-6.,-4.,14.6));
#21622=CARTESIAN_POINT('Origin',(-6.,-4.,14.6));
#21623=CARTESIAN_POINT('Origin',(-6.,-4.,12.1));
#21624=CARTESIAN_POINT('',(-7.05,-4.,12.1));
#21625=CARTESIAN_POINT('Origin',(-6.,-4.,12.1));
#21626=CARTESIAN_POINT('',(-7.05,-4.,15.1));
#21627=CARTESIAN_POINT('',(-7.05,-4.,12.1));
#21628=CARTESIAN_POINT('Origin',(-6.,-4.,15.1));
#21629=CARTESIAN_POINT('Origin',(-6.,-4.,12.1));
#21630=CARTESIAN_POINT('',(-6.625,-4.,12.1));
#21631=CARTESIAN_POINT('Origin',(-6.,-4.,12.1));
#21632=CARTESIAN_POINT('Origin',(-6.,-4.,14.6));
#21633=CARTESIAN_POINT('',(-8.,-4.,14.6));
#21634=CARTESIAN_POINT('Origin',(-6.,-4.,14.6));
#21635=CARTESIAN_POINT('Origin',(-6.,-4.,14.6));
#21636=CARTESIAN_POINT('',(-8.,-4.,15.1));
#21637=CARTESIAN_POINT('Origin',(-6.,-4.,15.1));
#21638=CARTESIAN_POINT('',(-8.,-4.,14.6));
#21639=CARTESIAN_POINT('Origin',(-6.,-4.,11.5));
#21640=CARTESIAN_POINT('',(-6.625,-4.,11.5));
#21641=CARTESIAN_POINT('',(-6.625,-4.,11.5));
#21642=CARTESIAN_POINT('Origin',(-6.,-4.,11.5));
#21643=CARTESIAN_POINT('Origin',(-6.,-4.,15.1));
#21644=CARTESIAN_POINT('Origin',(-6.,-4.,11.5));
#21645=CARTESIAN_POINT('',(0.,0.,0.));
#21646=CARTESIAN_POINT('Origin',(-7.13137084989848,2.86862915010152,14.));
#21647=CARTESIAN_POINT('',(-6.96707794165985,2.85337004454142,14.));
#21648=CARTESIAN_POINT('',(-7.14662995545858,3.03292205834015,14.));
#21649=CARTESIAN_POINT('Origin',(-6.,4.,14.));
#21650=CARTESIAN_POINT('Origin',(-7.13137084989848,2.86862915010152,14.));
#21651=CARTESIAN_POINT('Origin',(-7.13137084989848,2.86862915010152,14.));
#21652=CARTESIAN_POINT('',(-6.96707794165985,2.85337004454142,14.6));
#21653=CARTESIAN_POINT('',(-6.96707794165985,2.85337004454142,14.));
#21654=CARTESIAN_POINT('',(-7.29637084989848,2.86862915010152,14.6));
#21655=CARTESIAN_POINT('Origin',(-7.13137084989848,2.86862915010152,14.6));
#21656=CARTESIAN_POINT('',(-7.29637084989848,2.86862915010152,15.1));
#21657=CARTESIAN_POINT('',(-7.29637084989848,2.86862915010152,14.));
#21658=CARTESIAN_POINT('Origin',(-7.13137084989848,2.86862915010152,15.1));
#21659=CARTESIAN_POINT('',(-7.14662995545858,3.03292205834015,14.6));
#21660=CARTESIAN_POINT('Origin',(-7.13137084989848,2.86862915010152,14.6));
#21661=CARTESIAN_POINT('',(-7.14662995545858,3.03292205834015,14.));
#21662=CARTESIAN_POINT('Origin',(-7.13137084989848,5.13137084989848,14.));
#21663=CARTESIAN_POINT('',(-7.14662995545858,4.96707794165985,14.));
#21664=CARTESIAN_POINT('',(-6.96707794165985,5.14662995545858,14.));
#21665=CARTESIAN_POINT('Origin',(-6.,4.,14.));
#21666=CARTESIAN_POINT('Origin',(-7.13137084989848,5.13137084989848,14.));
#21667=CARTESIAN_POINT('Origin',(-7.13137084989848,5.13137084989848,14.));
#21668=CARTESIAN_POINT('',(-7.14662995545858,4.96707794165985,14.6));
#21669=CARTESIAN_POINT('',(-7.14662995545858,4.96707794165985,14.));
#21670=CARTESIAN_POINT('',(-7.29637084989848,5.13137084989848,14.6));
#21671=CARTESIAN_POINT('Origin',(-7.13137084989848,5.13137084989848,14.6));
#21672=CARTESIAN_POINT('',(-7.29637084989848,5.13137084989848,15.1));
#21673=CARTESIAN_POINT('',(-7.29637084989848,5.13137084989848,14.));
#21674=CARTESIAN_POINT('Origin',(-7.13137084989848,5.13137084989848,15.1));
#21675=CARTESIAN_POINT('',(-6.96707794165985,5.14662995545858,14.6));
#21676=CARTESIAN_POINT('Origin',(-7.13137084989848,5.13137084989848,14.6));
#21677=CARTESIAN_POINT('',(-6.96707794165985,5.14662995545858,14.));
#21678=CARTESIAN_POINT('Origin',(-4.86862915010152,5.13137084989848,14.));
#21679=CARTESIAN_POINT('',(-5.03292205834015,5.14662995545858,14.));
#21680=CARTESIAN_POINT('',(-4.85337004454142,4.96707794165985,14.));
#21681=CARTESIAN_POINT('Origin',(-6.,4.,14.));
#21682=CARTESIAN_POINT('',(-5.03362915010152,5.13137084989848,14.));
#21683=CARTESIAN_POINT('Origin',(-4.86862915010152,5.13137084989848,14.));
#21684=CARTESIAN_POINT('Origin',(-4.86862915010152,5.13137084989848,14.));
#21685=CARTESIAN_POINT('Origin',(-4.86862915010152,5.13137084989848,14.));
#21686=CARTESIAN_POINT('',(-5.03292205834015,5.14662995545858,14.6));
#21687=CARTESIAN_POINT('',(-5.03292205834015,5.14662995545858,14.));
#21688=CARTESIAN_POINT('',(-4.85337004454142,4.96707794165985,14.6));
#21689=CARTESIAN_POINT('Origin',(-4.86862915010152,5.13137084989848,14.6));
#21690=CARTESIAN_POINT('',(-4.85337004454142,4.96707794165985,14.));
#21691=CARTESIAN_POINT('',(-5.03362915010152,5.13137084989848,15.1));
#21692=CARTESIAN_POINT('',(-5.03362915010152,5.13137084989848,14.));
#21693=CARTESIAN_POINT('Origin',(-4.86862915010152,5.13137084989848,15.1));
#21694=CARTESIAN_POINT('Origin',(-4.86862915010152,2.86862915010152,14.));
#21695=CARTESIAN_POINT('',(-4.85337004454142,3.03292205834015,14.));
#21696=CARTESIAN_POINT('',(-5.03292205834015,2.85337004454142,14.));
#21697=CARTESIAN_POINT('Origin',(-6.,4.,14.));
#21698=CARTESIAN_POINT('',(-5.03362915010152,2.86862915010152,14.));
#21699=CARTESIAN_POINT('Origin',(-4.86862915010152,2.86862915010152,14.));
#21700=CARTESIAN_POINT('Origin',(-4.86862915010152,2.86862915010152,14.));
#21701=CARTESIAN_POINT('Origin',(-4.86862915010152,2.86862915010152,14.));
#21702=CARTESIAN_POINT('',(-4.85337004454142,3.03292205834015,14.6));
#21703=CARTESIAN_POINT('',(-4.85337004454142,3.03292205834015,14.));
#21704=CARTESIAN_POINT('',(-5.03292205834015,2.85337004454142,14.6));
#21705=CARTESIAN_POINT('Origin',(-4.86862915010152,2.86862915010152,14.6));
#21706=CARTESIAN_POINT('',(-5.03292205834015,2.85337004454142,14.));
#21707=CARTESIAN_POINT('',(-5.03362915010152,2.86862915010152,15.1));
#21708=CARTESIAN_POINT('',(-5.03362915010152,2.86862915010152,14.));
#21709=CARTESIAN_POINT('Origin',(-4.86862915010152,2.86862915010152,15.1));
#21710=CARTESIAN_POINT('Origin',(-6.,4.,11.5));
#21711=CARTESIAN_POINT('',(-7.5,4.,14.6));
#21712=CARTESIAN_POINT('Origin',(-6.,4.,14.6));
#21713=CARTESIAN_POINT('',(-7.5,4.,11.5));
#21714=CARTESIAN_POINT('',(-7.5,4.,11.5));
#21715=CARTESIAN_POINT('Origin',(-6.,4.,11.5));
#21716=CARTESIAN_POINT('Origin',(-6.,4.,14.6));
#21717=CARTESIAN_POINT('Origin',(-6.,4.,14.6));
#21718=CARTESIAN_POINT('Origin',(-6.,4.,14.6));
#21719=CARTESIAN_POINT('Origin',(-6.,4.,14.6));
#21720=CARTESIAN_POINT('Origin',(-6.,4.,12.1));
#21721=CARTESIAN_POINT('',(-7.05,4.,12.1));
#21722=CARTESIAN_POINT('Origin',(-6.,4.,12.1));
#21723=CARTESIAN_POINT('',(-7.05,4.,15.1));
#21724=CARTESIAN_POINT('',(-7.05,4.,12.1));
#21725=CARTESIAN_POINT('Origin',(-6.,4.,15.1));
#21726=CARTESIAN_POINT('Origin',(-6.,4.,12.1));
#21727=CARTESIAN_POINT('',(-6.625,4.,12.1));
#21728=CARTESIAN_POINT('Origin',(-6.,4.,12.1));
#21729=CARTESIAN_POINT('Origin',(-6.,4.,14.6));
#21730=CARTESIAN_POINT('',(-8.,4.,14.6));
#21731=CARTESIAN_POINT('Origin',(-6.,4.,14.6));
#21732=CARTESIAN_POINT('Origin',(-6.,4.,14.6));
#21733=CARTESIAN_POINT('',(-8.,4.,15.1));
#21734=CARTESIAN_POINT('Origin',(-6.,4.,15.1));
#21735=CARTESIAN_POINT('',(-8.,4.,14.6));
#21736=CARTESIAN_POINT('Origin',(-6.,4.,11.5));
#21737=CARTESIAN_POINT('',(-6.625,4.,11.5));
#21738=CARTESIAN_POINT('',(-6.625,4.,11.5));
#21739=CARTESIAN_POINT('Origin',(-6.,4.,11.5));
#21740=CARTESIAN_POINT('Origin',(-6.,4.,15.1));
#21741=CARTESIAN_POINT('Origin',(-6.,4.,11.5));
#21742=CARTESIAN_POINT('',(0.,0.,0.));
#21743=CARTESIAN_POINT('Origin',(4.86862915010152,-5.13137084989848,14.));
#21744=CARTESIAN_POINT('',(5.03292205834015,-5.14662995545858,14.));
#21745=CARTESIAN_POINT('',(4.85337004454142,-4.96707794165985,14.));
#21746=CARTESIAN_POINT('Origin',(6.,-4.,14.));
#21747=CARTESIAN_POINT('Origin',(4.86862915010152,-5.13137084989848,14.));
#21748=CARTESIAN_POINT('Origin',(4.86862915010152,-5.13137084989848,14.));
#21749=CARTESIAN_POINT('',(5.03292205834015,-5.14662995545858,14.6));
#21750=CARTESIAN_POINT('',(5.03292205834015,-5.14662995545858,14.));
#21751=CARTESIAN_POINT('',(4.70362915010152,-5.13137084989848,14.6));
#21752=CARTESIAN_POINT('Origin',(4.86862915010152,-5.13137084989848,14.6));
#21753=CARTESIAN_POINT('',(4.70362915010152,-5.13137084989848,15.1));
#21754=CARTESIAN_POINT('',(4.70362915010152,-5.13137084989848,14.));
#21755=CARTESIAN_POINT('Origin',(4.86862915010152,-5.13137084989848,15.1));
#21756=CARTESIAN_POINT('',(4.85337004454142,-4.96707794165985,14.6));
#21757=CARTESIAN_POINT('Origin',(4.86862915010152,-5.13137084989848,14.6));
#21758=CARTESIAN_POINT('',(4.85337004454142,-4.96707794165985,14.));
#21759=CARTESIAN_POINT('Origin',(4.86862915010152,-2.86862915010152,14.));
#21760=CARTESIAN_POINT('',(4.85337004454142,-3.03292205834015,14.));
#21761=CARTESIAN_POINT('',(5.03292205834015,-2.85337004454142,14.));
#21762=CARTESIAN_POINT('Origin',(6.,-4.,14.));
#21763=CARTESIAN_POINT('Origin',(4.86862915010152,-2.86862915010152,14.));
#21764=CARTESIAN_POINT('Origin',(4.86862915010152,-2.86862915010152,14.));
#21765=CARTESIAN_POINT('',(4.85337004454142,-3.03292205834015,14.6));
#21766=CARTESIAN_POINT('',(4.85337004454142,-3.03292205834015,14.));
#21767=CARTESIAN_POINT('',(4.70362915010152,-2.86862915010152,14.6));
#21768=CARTESIAN_POINT('Origin',(4.86862915010152,-2.86862915010152,14.6));
#21769=CARTESIAN_POINT('',(4.70362915010152,-2.86862915010152,15.1));
#21770=CARTESIAN_POINT('',(4.70362915010152,-2.86862915010152,14.));
#21771=CARTESIAN_POINT('Origin',(4.86862915010152,-2.86862915010152,15.1));
#21772=CARTESIAN_POINT('',(5.03292205834015,-2.85337004454142,14.6));
#21773=CARTESIAN_POINT('Origin',(4.86862915010152,-2.86862915010152,14.6));
#21774=CARTESIAN_POINT('',(5.03292205834015,-2.85337004454142,14.));
#21775=CARTESIAN_POINT('Origin',(7.13137084989848,-2.86862915010152,14.));
#21776=CARTESIAN_POINT('',(6.96707794165985,-2.85337004454142,14.));
#21777=CARTESIAN_POINT('',(7.14662995545858,-3.03292205834015,14.));
#21778=CARTESIAN_POINT('Origin',(6.,-4.,14.));
#21779=CARTESIAN_POINT('',(6.96637084989848,-2.86862915010152,14.));
#21780=CARTESIAN_POINT('Origin',(7.13137084989848,-2.86862915010152,14.));
#21781=CARTESIAN_POINT('Origin',(7.13137084989848,-2.86862915010152,14.));
#21782=CARTESIAN_POINT('Origin',(7.13137084989848,-2.86862915010152,14.));
#21783=CARTESIAN_POINT('',(6.96707794165985,-2.85337004454142,14.6));
#21784=CARTESIAN_POINT('',(6.96707794165985,-2.85337004454142,14.));
#21785=CARTESIAN_POINT('',(7.14662995545858,-3.03292205834015,14.6));
#21786=CARTESIAN_POINT('Origin',(7.13137084989848,-2.86862915010152,14.6));
#21787=CARTESIAN_POINT('',(7.14662995545858,-3.03292205834015,14.));
#21788=CARTESIAN_POINT('',(6.96637084989848,-2.86862915010152,15.1));
#21789=CARTESIAN_POINT('',(6.96637084989848,-2.86862915010152,14.));
#21790=CARTESIAN_POINT('Origin',(7.13137084989848,-2.86862915010152,15.1));
#21791=CARTESIAN_POINT('Origin',(7.13137084989848,-5.13137084989848,14.));
#21792=CARTESIAN_POINT('',(7.14662995545858,-4.96707794165985,14.));
#21793=CARTESIAN_POINT('',(6.96707794165985,-5.14662995545858,14.));
#21794=CARTESIAN_POINT('Origin',(6.,-4.,14.));
#21795=CARTESIAN_POINT('',(6.96637084989848,-5.13137084989848,14.));
#21796=CARTESIAN_POINT('Origin',(7.13137084989848,-5.13137084989848,14.));
#21797=CARTESIAN_POINT('Origin',(7.13137084989848,-5.13137084989848,14.));
#21798=CARTESIAN_POINT('Origin',(7.13137084989848,-5.13137084989848,14.));
#21799=CARTESIAN_POINT('',(7.14662995545858,-4.96707794165985,14.6));
#21800=CARTESIAN_POINT('',(7.14662995545858,-4.96707794165985,14.));
#21801=CARTESIAN_POINT('',(6.96707794165985,-5.14662995545858,14.6));
#21802=CARTESIAN_POINT('Origin',(7.13137084989848,-5.13137084989848,14.6));
#21803=CARTESIAN_POINT('',(6.96707794165985,-5.14662995545858,14.));
#21804=CARTESIAN_POINT('',(6.96637084989848,-5.13137084989848,15.1));
#21805=CARTESIAN_POINT('',(6.96637084989848,-5.13137084989848,14.));
#21806=CARTESIAN_POINT('Origin',(7.13137084989848,-5.13137084989848,15.1));
#21807=CARTESIAN_POINT('Origin',(6.,-4.,11.5));
#21808=CARTESIAN_POINT('',(4.5,-4.,14.6));
#21809=CARTESIAN_POINT('Origin',(6.,-4.,14.6));
#21810=CARTESIAN_POINT('',(4.5,-4.,11.5));
#21811=CARTESIAN_POINT('',(4.5,-4.,11.5));
#21812=CARTESIAN_POINT('Origin',(6.,-4.,11.5));
#21813=CARTESIAN_POINT('Origin',(6.,-4.,14.6));
#21814=CARTESIAN_POINT('Origin',(6.,-4.,14.6));
#21815=CARTESIAN_POINT('Origin',(6.,-4.,14.6));
#21816=CARTESIAN_POINT('Origin',(6.,-4.,14.6));
#21817=CARTESIAN_POINT('Origin',(6.,-4.,12.1));
#21818=CARTESIAN_POINT('',(4.95,-4.,12.1));
#21819=CARTESIAN_POINT('Origin',(6.,-4.,12.1));
#21820=CARTESIAN_POINT('',(4.95,-4.,15.1));
#21821=CARTESIAN_POINT('',(4.95,-4.,12.1));
#21822=CARTESIAN_POINT('Origin',(6.,-4.,15.1));
#21823=CARTESIAN_POINT('Origin',(6.,-4.,12.1));
#21824=CARTESIAN_POINT('',(5.375,-4.,12.1));
#21825=CARTESIAN_POINT('Origin',(6.,-4.,12.1));
#21826=CARTESIAN_POINT('Origin',(6.,-4.,14.6));
#21827=CARTESIAN_POINT('',(4.,-4.,14.6));
#21828=CARTESIAN_POINT('Origin',(6.,-4.,14.6));
#21829=CARTESIAN_POINT('Origin',(6.,-4.,14.6));
#21830=CARTESIAN_POINT('',(4.,-4.,15.1));
#21831=CARTESIAN_POINT('Origin',(6.,-4.,15.1));
#21832=CARTESIAN_POINT('',(4.,-4.,14.6));
#21833=CARTESIAN_POINT('Origin',(6.,-4.,11.5));
#21834=CARTESIAN_POINT('',(5.375,-4.,11.5));
#21835=CARTESIAN_POINT('',(5.375,-4.,11.5));
#21836=CARTESIAN_POINT('Origin',(6.,-4.,11.5));
#21837=CARTESIAN_POINT('Origin',(6.,-4.,15.1));
#21838=CARTESIAN_POINT('Origin',(6.,-4.,11.5));
#21839=CARTESIAN_POINT('',(0.,0.,0.));
#21840=CARTESIAN_POINT('Origin',(4.86862915010152,2.86862915010152,14.));
#21841=CARTESIAN_POINT('',(5.03292205834015,2.85337004454142,14.));
#21842=CARTESIAN_POINT('',(4.85337004454142,3.03292205834015,14.));
#21843=CARTESIAN_POINT('Origin',(6.,4.,14.));
#21844=CARTESIAN_POINT('Origin',(4.86862915010152,2.86862915010152,14.));
#21845=CARTESIAN_POINT('Origin',(4.86862915010152,2.86862915010152,14.));
#21846=CARTESIAN_POINT('',(5.03292205834015,2.85337004454142,14.6));
#21847=CARTESIAN_POINT('',(5.03292205834015,2.85337004454142,14.));
#21848=CARTESIAN_POINT('',(4.70362915010152,2.86862915010152,14.6));
#21849=CARTESIAN_POINT('Origin',(4.86862915010152,2.86862915010152,14.6));
#21850=CARTESIAN_POINT('',(4.70362915010152,2.86862915010152,15.1));
#21851=CARTESIAN_POINT('',(4.70362915010152,2.86862915010152,14.));
#21852=CARTESIAN_POINT('Origin',(4.86862915010152,2.86862915010152,15.1));
#21853=CARTESIAN_POINT('',(4.85337004454142,3.03292205834015,14.6));
#21854=CARTESIAN_POINT('Origin',(4.86862915010152,2.86862915010152,14.6));
#21855=CARTESIAN_POINT('',(4.85337004454142,3.03292205834015,14.));
#21856=CARTESIAN_POINT('Origin',(4.86862915010152,5.13137084989848,14.));
#21857=CARTESIAN_POINT('',(4.85337004454142,4.96707794165985,14.));
#21858=CARTESIAN_POINT('',(5.03292205834015,5.14662995545858,14.));
#21859=CARTESIAN_POINT('Origin',(6.,4.,14.));
#21860=CARTESIAN_POINT('Origin',(4.86862915010152,5.13137084989848,14.));
#21861=CARTESIAN_POINT('Origin',(4.86862915010152,5.13137084989848,14.));
#21862=CARTESIAN_POINT('',(4.85337004454142,4.96707794165985,14.6));
#21863=CARTESIAN_POINT('',(4.85337004454142,4.96707794165985,14.));
#21864=CARTESIAN_POINT('',(4.70362915010152,5.13137084989848,14.6));
#21865=CARTESIAN_POINT('Origin',(4.86862915010152,5.13137084989848,14.6));
#21866=CARTESIAN_POINT('',(4.70362915010152,5.13137084989848,15.1));
#21867=CARTESIAN_POINT('',(4.70362915010152,5.13137084989848,14.));
#21868=CARTESIAN_POINT('Origin',(4.86862915010152,5.13137084989848,15.1));
#21869=CARTESIAN_POINT('',(5.03292205834015,5.14662995545858,14.6));
#21870=CARTESIAN_POINT('Origin',(4.86862915010152,5.13137084989848,14.6));
#21871=CARTESIAN_POINT('',(5.03292205834015,5.14662995545858,14.));
#21872=CARTESIAN_POINT('Origin',(7.13137084989848,5.13137084989848,14.));
#21873=CARTESIAN_POINT('',(6.96707794165985,5.14662995545858,14.));
#21874=CARTESIAN_POINT('',(7.14662995545858,4.96707794165985,14.));
#21875=CARTESIAN_POINT('Origin',(6.,4.,14.));
#21876=CARTESIAN_POINT('',(6.96637084989848,5.13137084989848,14.));
#21877=CARTESIAN_POINT('Origin',(7.13137084989848,5.13137084989848,14.));
#21878=CARTESIAN_POINT('Origin',(7.13137084989848,5.13137084989848,14.));
#21879=CARTESIAN_POINT('Origin',(7.13137084989848,5.13137084989848,14.));
#21880=CARTESIAN_POINT('',(6.96707794165985,5.14662995545858,14.6));
#21881=CARTESIAN_POINT('',(6.96707794165985,5.14662995545858,14.));
#21882=CARTESIAN_POINT('',(7.14662995545858,4.96707794165985,14.6));
#21883=CARTESIAN_POINT('Origin',(7.13137084989848,5.13137084989848,14.6));
#21884=CARTESIAN_POINT('',(7.14662995545858,4.96707794165985,14.));
#21885=CARTESIAN_POINT('',(6.96637084989848,5.13137084989848,15.1));
#21886=CARTESIAN_POINT('',(6.96637084989848,5.13137084989848,14.));
#21887=CARTESIAN_POINT('Origin',(7.13137084989848,5.13137084989848,15.1));
#21888=CARTESIAN_POINT('Origin',(7.13137084989848,2.86862915010152,14.));
#21889=CARTESIAN_POINT('',(7.14662995545858,3.03292205834015,14.));
#21890=CARTESIAN_POINT('',(6.96707794165985,2.85337004454142,14.));
#21891=CARTESIAN_POINT('Origin',(6.,4.,14.));
#21892=CARTESIAN_POINT('',(6.96637084989848,2.86862915010152,14.));
#21893=CARTESIAN_POINT('Origin',(7.13137084989848,2.86862915010152,14.));
#21894=CARTESIAN_POINT('Origin',(7.13137084989848,2.86862915010152,14.));
#21895=CARTESIAN_POINT('Origin',(7.13137084989848,2.86862915010152,14.));
#21896=CARTESIAN_POINT('',(7.14662995545858,3.03292205834015,14.6));
#21897=CARTESIAN_POINT('',(7.14662995545858,3.03292205834015,14.));
#21898=CARTESIAN_POINT('',(6.96707794165985,2.85337004454142,14.6));
#21899=CARTESIAN_POINT('Origin',(7.13137084989848,2.86862915010152,14.6));
#21900=CARTESIAN_POINT('',(6.96707794165985,2.85337004454142,14.));
#21901=CARTESIAN_POINT('',(6.96637084989848,2.86862915010152,15.1));
#21902=CARTESIAN_POINT('',(6.96637084989848,2.86862915010152,14.));
#21903=CARTESIAN_POINT('Origin',(7.13137084989848,2.86862915010152,15.1));
#21904=CARTESIAN_POINT('Origin',(6.,4.,11.5));
#21905=CARTESIAN_POINT('',(4.5,4.,14.6));
#21906=CARTESIAN_POINT('Origin',(6.,4.,14.6));
#21907=CARTESIAN_POINT('',(4.5,4.,11.5));
#21908=CARTESIAN_POINT('',(4.5,4.,11.5));
#21909=CARTESIAN_POINT('Origin',(6.,4.,11.5));
#21910=CARTESIAN_POINT('Origin',(6.,4.,14.6));
#21911=CARTESIAN_POINT('Origin',(6.,4.,14.6));
#21912=CARTESIAN_POINT('Origin',(6.,4.,14.6));
#21913=CARTESIAN_POINT('Origin',(6.,4.,14.6));
#21914=CARTESIAN_POINT('Origin',(6.,4.,12.1));
#21915=CARTESIAN_POINT('',(4.95,4.,12.1));
#21916=CARTESIAN_POINT('Origin',(6.,4.,12.1));
#21917=CARTESIAN_POINT('',(4.95,4.,15.1));
#21918=CARTESIAN_POINT('',(4.95,4.,12.1));
#21919=CARTESIAN_POINT('Origin',(6.,4.,15.1));
#21920=CARTESIAN_POINT('Origin',(6.,4.,12.1));
#21921=CARTESIAN_POINT('',(5.375,4.,12.1));
#21922=CARTESIAN_POINT('Origin',(6.,4.,12.1));
#21923=CARTESIAN_POINT('Origin',(6.,4.,14.6));
#21924=CARTESIAN_POINT('',(4.,4.,14.6));
#21925=CARTESIAN_POINT('Origin',(6.,4.,14.6));
#21926=CARTESIAN_POINT('Origin',(6.,4.,14.6));
#21927=CARTESIAN_POINT('',(4.,4.,15.1));
#21928=CARTESIAN_POINT('Origin',(6.,4.,15.1));
#21929=CARTESIAN_POINT('',(4.,4.,14.6));
#21930=CARTESIAN_POINT('Origin',(6.,4.,11.5));
#21931=CARTESIAN_POINT('',(5.375,4.,11.5));
#21932=CARTESIAN_POINT('',(5.375,4.,11.5));
#21933=CARTESIAN_POINT('Origin',(6.,4.,11.5));
#21934=CARTESIAN_POINT('Origin',(6.,4.,15.1));
#21935=CARTESIAN_POINT('Origin',(6.,4.,11.5));
#21936=CARTESIAN_POINT('',(0.,0.,0.));
#21937=CARTESIAN_POINT('Origin',(0.,-1.,14.4));
#21938=CARTESIAN_POINT('',(-0.165,-1.,14.5));
#21939=CARTESIAN_POINT('Origin',(0.,-1.,14.5));
#21940=CARTESIAN_POINT('',(-0.165,-1.,15.1));
#21941=CARTESIAN_POINT('',(-0.165,-1.,14.4));
#21942=CARTESIAN_POINT('Origin',(0.,-1.,15.1));
#21943=CARTESIAN_POINT('Origin',(1.,0.,14.4));
#21944=CARTESIAN_POINT('',(0.835,-2.02066721859313E-17,14.5));
#21945=CARTESIAN_POINT('Origin',(1.,0.,14.5));
#21946=CARTESIAN_POINT('',(0.835,2.02066721859313E-17,15.1));
#21947=CARTESIAN_POINT('',(0.835,-2.02066721859313E-17,14.4));
#21948=CARTESIAN_POINT('Origin',(1.,0.,15.1));
#21949=CARTESIAN_POINT('Origin',(-1.,0.,14.4));
#21950=CARTESIAN_POINT('',(-1.165,-2.02066721859313E-17,14.5));
#21951=CARTESIAN_POINT('Origin',(-1.,0.,14.5));
#21952=CARTESIAN_POINT('',(-1.165,2.02066721859313E-17,15.1));
#21953=CARTESIAN_POINT('',(-1.165,-2.02066721859313E-17,14.4));
#21954=CARTESIAN_POINT('Origin',(-1.,0.,15.1));
#21955=CARTESIAN_POINT('Origin',(0.,1.,14.4));
#21956=CARTESIAN_POINT('',(-0.165,1.,14.5));
#21957=CARTESIAN_POINT('Origin',(0.,1.,14.5));
#21958=CARTESIAN_POINT('',(-0.165,1.,15.1));
#21959=CARTESIAN_POINT('',(-0.165,1.,14.4));
#21960=CARTESIAN_POINT('Origin',(0.,1.,15.1));
#21961=CARTESIAN_POINT('Origin',(0.,0.,14.5));
#21962=CARTESIAN_POINT('',(-1.5,-1.83697019872103E-16,14.5));
#21963=CARTESIAN_POINT('Origin',(0.,0.,14.5));
#21964=CARTESIAN_POINT('',(-0.5,6.12323399573677E-17,14.5));
#21965=CARTESIAN_POINT('Origin',(0.,0.,14.5));
#21966=CARTESIAN_POINT('Origin',(0.,0.,14.5));
#21967=CARTESIAN_POINT('',(-1.5,-1.83697019872103E-16,15.1));
#21968=CARTESIAN_POINT('Origin',(0.,0.,15.1));
#21969=CARTESIAN_POINT('',(-1.5,-1.83697019872103E-16,14.5));
#21970=CARTESIAN_POINT('Origin',(0.,0.,8.));
#21971=CARTESIAN_POINT('',(-0.5,-6.12323399573677E-17,8.));
#21972=CARTESIAN_POINT('',(-0.5,-6.12323399573677E-17,8.));
#21973=CARTESIAN_POINT('Origin',(0.,0.,8.));
#21974=CARTESIAN_POINT('Origin',(0.,0.,15.1));
#21975=CARTESIAN_POINT('Origin',(0.,0.,8.));
#21976=CARTESIAN_POINT('',(0.,0.,0.));
#21977=CARTESIAN_POINT('',(0.,0.,0.));
#21978=CARTESIAN_POINT('Origin',(0.75,1.2,0.));
#21979=CARTESIAN_POINT('',(0.885663593019381,1.2,-0.16));
#21980=CARTESIAN_POINT('',(0.885663593019381,1.2,0.16));
#21981=CARTESIAN_POINT('Origin',(0.,1.2,0.));
#21982=CARTESIAN_POINT('',(0.93,1.2,-0.16));
#21983=CARTESIAN_POINT('',(0.93,1.2,-0.16));
#21984=CARTESIAN_POINT('',(0.93,1.2,0.16));
#21985=CARTESIAN_POINT('',(0.93,1.2,0.16));
#21986=CARTESIAN_POINT('',(0.57,1.2,0.16));
#21987=CARTESIAN_POINT('Origin',(0.57,0.,0.16));
#21988=CARTESIAN_POINT('',(0.885663593019381,-1.2,0.16));
#21989=CARTESIAN_POINT('',(0.885663593019381,0.,0.16));
#21990=CARTESIAN_POINT('',(0.93,-1.2,0.16));
#21991=CARTESIAN_POINT('',(0.93,0.,0.16));
#21992=CARTESIAN_POINT('',(0.57,-1.2,0.16));
#21993=CARTESIAN_POINT('Origin',(0.75,-1.2,0.));
#21994=CARTESIAN_POINT('',(0.885663593019381,-1.2,-0.16));
#21995=CARTESIAN_POINT('Origin',(0.,-1.2,0.));
#21996=CARTESIAN_POINT('',(0.93,-1.2,-0.16));
#21997=CARTESIAN_POINT('',(0.93,-1.2,0.16));
#21998=CARTESIAN_POINT('',(0.93,-1.2,-0.16));
#21999=CARTESIAN_POINT('Origin',(0.93,0.,-0.16));
#22000=CARTESIAN_POINT('',(0.885663593019381,0.,-0.16));
#22001=CARTESIAN_POINT('',(0.93,0.,-0.16));
#22002=CARTESIAN_POINT('Origin',(0.93,0.,0.16));
#22003=CARTESIAN_POINT('Origin',(1.05,1.5,0.));
#22004=CARTESIAN_POINT('',(-1.05,1.5,-1.28587913910472E-16));
#22005=CARTESIAN_POINT('Origin',(0.,1.5,0.));
#22006=CARTESIAN_POINT('',(-0.9,1.5,-1.10218211923262E-16));
#22007=CARTESIAN_POINT('Origin',(0.,1.5,0.));
#22008=CARTESIAN_POINT('Origin',(0.,1.315,0.));
#22009=CARTESIAN_POINT('',(-1.05,1.13,-1.28587913910472E-16));
#22010=CARTESIAN_POINT('Origin',(0.,1.13,0.));
#22011=CARTESIAN_POINT('',(-1.05,1.315,-1.28587913910472E-16));
#22012=CARTESIAN_POINT('Origin',(1.,1.13,0.));
#22013=CARTESIAN_POINT('',(-1.,1.13,-1.22464679914735E-16));
#22014=CARTESIAN_POINT('Origin',(0.,1.13,0.));
#22015=CARTESIAN_POINT('Origin',(0.,1.065,0.));
#22016=CARTESIAN_POINT('',(-1.,1.,-1.22464679914735E-16));
#22017=CARTESIAN_POINT('Origin',(0.,1.,0.));
#22018=CARTESIAN_POINT('',(-1.,1.065,-1.22464679914735E-16));
#22019=CARTESIAN_POINT('Origin',(1.05,1.,0.));
#22020=CARTESIAN_POINT('',(-1.05,1.,-1.28587913910472E-16));
#22021=CARTESIAN_POINT('Origin',(0.,1.,0.));
#22022=CARTESIAN_POINT('Origin',(0.,0.,0.));
#22023=CARTESIAN_POINT('',(-1.05,-1.,-1.28587913910472E-16));
#22024=CARTESIAN_POINT('Origin',(0.,-1.,0.));
#22025=CARTESIAN_POINT('',(-1.05,0.,-1.28587913910472E-16));
#22026=CARTESIAN_POINT('Origin',(1.,-1.,0.));
#22027=CARTESIAN_POINT('',(-1.,-1.,-1.22464679914735E-16));
#22028=CARTESIAN_POINT('Origin',(0.,-1.,0.));
#22029=CARTESIAN_POINT('Origin',(0.,-1.065,0.));
#22030=CARTESIAN_POINT('',(-1.,-1.13,-1.22464679914735E-16));
#22031=CARTESIAN_POINT('Origin',(0.,-1.13,0.));
#22032=CARTESIAN_POINT('',(-1.,-1.065,-1.22464679914735E-16));
#22033=CARTESIAN_POINT('Origin',(1.05,-1.13,0.));
#22034=CARTESIAN_POINT('',(-1.05,-1.13,-1.28587913910472E-16));
#22035=CARTESIAN_POINT('Origin',(0.,-1.13,0.));
#22036=CARTESIAN_POINT('Origin',(0.,-1.315,0.));
#22037=CARTESIAN_POINT('',(-1.05,-1.5,-1.28587913910472E-16));
#22038=CARTESIAN_POINT('Origin',(0.,-1.5,0.));
#22039=CARTESIAN_POINT('',(-1.05,-1.315,-1.28587913910472E-16));
#22040=CARTESIAN_POINT('Origin',(0.9,-1.5,0.));
#22041=CARTESIAN_POINT('',(-0.9,-1.5,-1.10218211923262E-16));
#22042=CARTESIAN_POINT('Origin',(0.,-1.5,0.));
#22043=CARTESIAN_POINT('Origin',(0.,0.,0.));
#22044=CARTESIAN_POINT('',(-0.9,0.,-1.10218211923262E-16));
#22045=CARTESIAN_POINT('',(0.,0.,0.));
#22046=CARTESIAN_POINT('Origin',(0.75,1.2,0.));
#22047=CARTESIAN_POINT('',(0.880582193778639,1.2,0.16));
#22048=CARTESIAN_POINT('',(0.880582193778639,1.2,-0.16));
#22049=CARTESIAN_POINT('Origin',(0.,1.2,0.));
#22050=CARTESIAN_POINT('',(0.583459510163302,1.2,0.16));
#22051=CARTESIAN_POINT('',(0.57,1.2,0.16));
#22052=CARTESIAN_POINT('',(0.583459510163302,1.2,-0.16));
#22053=CARTESIAN_POINT('Origin',(0.,1.2,0.));
#22054=CARTESIAN_POINT('',(0.93,1.2,-0.16));
#22055=CARTESIAN_POINT('Origin',(0.93,0.,-0.16));
#22056=CARTESIAN_POINT('',(0.880582193778639,-1.2,-0.16));
#22057=CARTESIAN_POINT('',(0.880582193778639,0.,-0.16));
#22058=CARTESIAN_POINT('',(0.583459510163302,-1.2,-0.16));
#22059=CARTESIAN_POINT('',(0.583459510163302,0.,-0.16));
#22060=CARTESIAN_POINT('',(0.93,-1.2,-0.16));
#22061=CARTESIAN_POINT('Origin',(0.75,-1.2,0.));
#22062=CARTESIAN_POINT('',(0.880582193778639,-1.2,0.16));
#22063=CARTESIAN_POINT('Origin',(0.,-1.2,0.));
#22064=CARTESIAN_POINT('',(0.583459510163302,-1.2,0.16));
#22065=CARTESIAN_POINT('Origin',(0.,-1.2,0.));
#22066=CARTESIAN_POINT('',(0.57,-1.2,0.16));
#22067=CARTESIAN_POINT('Origin',(0.57,0.,0.16));
#22068=CARTESIAN_POINT('',(0.880582193778639,0.,0.16));
#22069=CARTESIAN_POINT('',(0.583459510163302,0.,0.16));
#22070=CARTESIAN_POINT('Origin',(0.895,1.35,0.));
#22071=CARTESIAN_POINT('',(-0.895,1.35,-1.09605888523688E-16));
#22072=CARTESIAN_POINT('Origin',(0.,1.35,0.));
#22073=CARTESIAN_POINT('',(-0.605,1.35,-7.40911313484149E-17));
#22074=CARTESIAN_POINT('Origin',(0.,1.35,0.));
#22075=CARTESIAN_POINT('Origin',(0.,0.,0.));
#22076=CARTESIAN_POINT('',(-0.895,-1.35,-1.09605888523688E-16));
#22077=CARTESIAN_POINT('Origin',(0.,-1.35,0.));
#22078=CARTESIAN_POINT('',(-0.895,0.,-1.09605888523688E-16));
#22079=CARTESIAN_POINT('Origin',(0.605,-1.35,0.));
#22080=CARTESIAN_POINT('',(-0.605,-1.35,-7.40911313484149E-17));
#22081=CARTESIAN_POINT('Origin',(0.,-1.35,0.));
#22082=CARTESIAN_POINT('Origin',(0.,0.,0.));
#22083=CARTESIAN_POINT('',(-0.605,0.,-7.40911313484149E-17));
#22084=CARTESIAN_POINT('',(0.,0.,0.));
#22085=CARTESIAN_POINT('',(0.,0.,0.));
#22086=CARTESIAN_POINT('',(0.,0.,0.));
#22087=CARTESIAN_POINT('Origin',(0.3,0.4,0.));
#22088=CARTESIAN_POINT('',(-0.3,0.4,-3.67394039744206E-17));
#22089=CARTESIAN_POINT('Origin',(0.,0.4,0.));
#22090=CARTESIAN_POINT('Origin',(0.,0.375,0.));
#22091=CARTESIAN_POINT('',(-0.35,0.35,-4.28626379701573E-17));
#22092=CARTESIAN_POINT('Origin',(0.,0.35,0.));
#22093=CARTESIAN_POINT('',(-0.325,0.375,-3.9801020972289E-17));
#22094=CARTESIAN_POINT('Origin',(0.,0.19,0.));
#22095=CARTESIAN_POINT('',(-0.35,0.03,-4.28626379701574E-17));
#22096=CARTESIAN_POINT('Origin',(0.,0.03,0.));
#22097=CARTESIAN_POINT('',(-0.35,0.19,-4.28626379701574E-17));
#22098=CARTESIAN_POINT('Origin',(0.,0.0149999999999999,0.));
#22099=CARTESIAN_POINT('',(-0.32,-3.29597460435593E-17,-3.91886975727153E-17));
#22100=CARTESIAN_POINT('Origin',(0.,0.,0.));
#22101=CARTESIAN_POINT('',(-0.335,0.0149999999999999,-4.10256677714363E-17));
#22102=CARTESIAN_POINT('Origin',(0.22,0.,0.));
#22103=CARTESIAN_POINT('',(-0.22,-6.93889390390723E-18,-2.69422295812418E-17));
#22104=CARTESIAN_POINT('Origin',(0.,0.,0.));
#22105=CARTESIAN_POINT('Origin',(0.,-0.02,0.));
#22106=CARTESIAN_POINT('',(-0.1954,-0.0492,2.39295984553393E-17));
#22107=CARTESIAN_POINT('Origin',(0.,-0.0492,0.));
#22108=CARTESIAN_POINT('',(-0.21,-0.02,-2.57175827820944E-17));
#22109=CARTESIAN_POINT('Origin',(0.,-0.8,0.));
#22110=CARTESIAN_POINT('',(-0.1954,-1.5646,2.39295984553393E-17));
#22111=CARTESIAN_POINT('Origin',(0.,-1.5646,0.));
#22112=CARTESIAN_POINT('',(-0.1954,-0.8,-2.39295984553393E-17));
#22113=CARTESIAN_POINT('Origin',(0.,-1.58,0.));
#22114=CARTESIAN_POINT('',(-0.16,-1.6,-1.95943487863577E-17));
#22115=CARTESIAN_POINT('Origin',(0.,-1.6,0.));
#22116=CARTESIAN_POINT('',(-0.18,-1.58,-2.20436423846524E-17));
#22117=CARTESIAN_POINT('Origin',(0.,-1.6,0.));
#22118=CARTESIAN_POINT('Origin',(0.0866025403784439,-0.4,-0.15));
#22119=CARTESIAN_POINT('',(0.173205080756888,-0.4,0.));
#22120=CARTESIAN_POINT('',(0.0866025403784439,-0.4,-0.15));
#22121=CARTESIAN_POINT('',(0.173205080756888,-0.4,0.));
#22122=CARTESIAN_POINT('',(0.0866025403784439,-0.64,-0.15));
#22123=CARTESIAN_POINT('',(0.0866025403784439,-0.4,-0.15));
#22124=CARTESIAN_POINT('',(0.173205080756888,-0.64,0.));
#22125=CARTESIAN_POINT('',(0.173205080756888,-0.64,0.));
#22126=CARTESIAN_POINT('',(0.173205080756888,-0.4,0.));
#22127=CARTESIAN_POINT('Origin',(-0.0866025403784438,-0.4,-0.15));
#22128=CARTESIAN_POINT('',(-0.0866025403784438,-0.4,-0.15));
#22129=CARTESIAN_POINT('',(0.0866025403784439,-0.4,-0.15));
#22130=CARTESIAN_POINT('',(-0.0866025403784438,-0.64,-0.15));
#22131=CARTESIAN_POINT('',(-0.0866025403784438,-0.4,-0.15));
#22132=CARTESIAN_POINT('',(0.0866025403784439,-0.64,-0.15));
#22133=CARTESIAN_POINT('Origin',(-0.173205080756888,-0.4,-2.77555756156289E-17));
#22134=CARTESIAN_POINT('',(-0.173205080756888,-0.4,-2.12115047744981E-17));
#22135=CARTESIAN_POINT('',(-0.0866025403784438,-0.4,-0.15));
#22136=CARTESIAN_POINT('',(-0.173205080756888,-0.64,-2.77555756156289E-17));
#22137=CARTESIAN_POINT('',(-0.173205080756888,-0.4,-2.12115047744981E-17));
#22138=CARTESIAN_POINT('',(-0.0866025403784438,-0.64,-0.15));
#22139=CARTESIAN_POINT('Origin',(-0.0866025403784439,-0.4,0.15));
#22140=CARTESIAN_POINT('',(-0.0866025403784439,-0.4,0.15));
#22141=CARTESIAN_POINT('',(-0.173205080756888,-0.4,-2.12115047744981E-17));
#22142=CARTESIAN_POINT('',(-0.0866025403784439,-0.64,0.15));
#22143=CARTESIAN_POINT('',(-0.0866025403784439,-0.4,0.15));
#22144=CARTESIAN_POINT('',(-0.173205080756888,-0.64,-2.12115047744981E-17));
#22145=CARTESIAN_POINT('Origin',(0.0866025403784439,-0.4,0.15));
#22146=CARTESIAN_POINT('',(0.0866025403784439,-0.4,0.15));
#22147=CARTESIAN_POINT('',(-0.0866025403784439,-0.4,0.15));
#22148=CARTESIAN_POINT('',(0.0866025403784439,-0.64,0.15));
#22149=CARTESIAN_POINT('',(0.0866025403784439,-0.4,0.15));
#22150=CARTESIAN_POINT('',(-0.0866025403784439,-0.64,0.15));
#22151=CARTESIAN_POINT('Origin',(0.173205080756888,-0.4,0.));
#22152=CARTESIAN_POINT('',(0.0866025403784439,-0.4,0.15));
#22153=CARTESIAN_POINT('',(0.0866025403784439,-0.64,0.15));
#22154=CARTESIAN_POINT('Origin',(0.,-0.4,-2.77555756156289E-17));
#22155=CARTESIAN_POINT('Origin',(0.,-0.64,-2.77555756156289E-17));
#22156=CARTESIAN_POINT('',(0.,0.,0.));
#22157=CARTESIAN_POINT('',(0.,0.,0.));
#22158=CARTESIAN_POINT('',(0.,0.,0.));
#22159=CARTESIAN_POINT('',(0.,0.,0.));
#22160=CARTESIAN_POINT('',(0.,0.,0.));
#22161=CARTESIAN_POINT('',(0.,0.,0.));
#22162=CARTESIAN_POINT('',(0.,0.,0.));
#22163=CARTESIAN_POINT('',(0.,0.,0.));
#22164=CARTESIAN_POINT('',(0.,0.,0.));
#22165=CARTESIAN_POINT('',(0.,0.,0.));
#22166=CARTESIAN_POINT('',(0.,0.,0.));
#22167=CARTESIAN_POINT('',(0.,0.,0.));
#22168=CARTESIAN_POINT('',(0.,0.,0.));
#22169=CARTESIAN_POINT('',(0.,0.,0.));
#22170=CARTESIAN_POINT('',(0.,0.,0.));
#22171=CARTESIAN_POINT('',(0.,0.,0.));
#22172=CARTESIAN_POINT('',(0.,0.,0.));
#22173=CARTESIAN_POINT('',(0.,0.,0.));
#22174=CARTESIAN_POINT('',(0.,0.,0.));
#22175=CARTESIAN_POINT('',(0.,0.,0.));
#22176=CARTESIAN_POINT('',(0.,0.,0.));
#22177=CARTESIAN_POINT('',(0.,0.,0.));
#22178=CARTESIAN_POINT('',(0.,0.,0.));
#22179=CARTESIAN_POINT('',(0.,0.,0.));
#22180=CARTESIAN_POINT('',(0.,0.,0.));
#22181=CARTESIAN_POINT('',(0.,0.,0.));
#22182=CARTESIAN_POINT('',(0.,0.,0.));
#22183=CARTESIAN_POINT('',(0.,0.,0.));
#22184=CARTESIAN_POINT('',(0.,0.,0.));
#22185=CARTESIAN_POINT('',(0.,0.,0.));
#22186=CARTESIAN_POINT('',(0.,0.,0.));
#22187=CARTESIAN_POINT('',(0.,0.,0.));
#22188=CARTESIAN_POINT('',(0.,0.,0.));
#22189=CARTESIAN_POINT('',(-9.5,10.,-1.2));
#22190=CARTESIAN_POINT('',(-9.5,10.,31.5));
#22191=CARTESIAN_POINT('',(-9.5,11.,-1.2));
#22192=CARTESIAN_POINT('',(-9.5,11.,31.5));
#22193=CARTESIAN_POINT('',(9.5,10.,-1.2));
#22194=CARTESIAN_POINT('',(9.5,10.,31.5));
#22195=CARTESIAN_POINT('',(9.5,11.,-1.2));
#22196=CARTESIAN_POINT('',(9.5,11.,31.5));
#22197=CARTESIAN_POINT('',(-6.,-4.,0.5));
#22198=CARTESIAN_POINT('',(-6.,-1.7,1.2));
#22199=CARTESIAN_POINT('',(-7.6,-2.3,1.2));
#22200=CARTESIAN_POINT('',(-4.4,-2.3,1.2));
#22201=CARTESIAN_POINT('',(-4.8,-5.05,1.2));
#22202=CARTESIAN_POINT('',(-7.6,-1.3,-1.2));
#22203=CARTESIAN_POINT('',(-4.4,-1.3,-1.2));
#22204=CARTESIAN_POINT('',(-6.,-1.7,29.8));
#22205=CARTESIAN_POINT('',(-7.6,-2.3,29.8));
#22206=CARTESIAN_POINT('',(-4.4,-2.3,29.8));
#22207=CARTESIAN_POINT('',(-4.8,-5.05,29.8));
#22208=CARTESIAN_POINT('',(-7.6,0.,31.5));
#22209=CARTESIAN_POINT('',(-4.4,0.,31.5));
#22210=CARTESIAN_POINT('',(-6.,4.,0.5));
#22211=CARTESIAN_POINT('',(-6.,6.3,1.2));
#22212=CARTESIAN_POINT('',(-7.6,5.7,1.2));
#22213=CARTESIAN_POINT('',(-4.4,5.7,1.2));
#22214=CARTESIAN_POINT('',(-4.8,2.95,1.2));
#22215=CARTESIAN_POINT('',(-7.6,6.7,-1.2));
#22216=CARTESIAN_POINT('',(-4.4,6.7,-1.2));
#22217=CARTESIAN_POINT('',(-6.,6.3,29.8));
#22218=CARTESIAN_POINT('',(-7.6,5.7,29.8));
#22219=CARTESIAN_POINT('',(-4.4,5.7,29.8));
#22220=CARTESIAN_POINT('',(-4.8,2.95,29.8));
#22221=CARTESIAN_POINT('',(-7.6,8.,31.5));
#22222=CARTESIAN_POINT('',(-4.4,8.,31.5));
#22223=CARTESIAN_POINT('',(6.,-4.,0.5));
#22224=CARTESIAN_POINT('',(6.,-1.7,1.2));
#22225=CARTESIAN_POINT('',(4.4,-2.3,1.2));
#22226=CARTESIAN_POINT('',(7.6,-2.3,1.2));
#22227=CARTESIAN_POINT('',(7.2,-5.05,1.2));
#22228=CARTESIAN_POINT('',(4.4,-1.3,-1.2));
#22229=CARTESIAN_POINT('',(7.6,-1.3,-1.2));
#22230=CARTESIAN_POINT('',(6.,-1.7,29.8));
#22231=CARTESIAN_POINT('',(4.4,-2.3,29.8));
#22232=CARTESIAN_POINT('',(7.6,-2.3,29.8));
#22233=CARTESIAN_POINT('',(7.2,-5.05,29.8));
#22234=CARTESIAN_POINT('',(4.4,0.,31.5));
#22235=CARTESIAN_POINT('',(7.6,0.,31.5));
#22236=CARTESIAN_POINT('',(6.,4.,0.5));
#22237=CARTESIAN_POINT('',(6.,6.3,1.2));
#22238=CARTESIAN_POINT('',(4.4,5.7,1.2));
#22239=CARTESIAN_POINT('',(7.6,5.7,1.2));
#22240=CARTESIAN_POINT('',(7.2,2.95,1.2));
#22241=CARTESIAN_POINT('',(4.4,6.7,-1.2));
#22242=CARTESIAN_POINT('',(7.6,6.7,-1.2));
#22243=CARTESIAN_POINT('',(6.,6.3,29.8));
#22244=CARTESIAN_POINT('',(4.4,5.7,29.8));
#22245=CARTESIAN_POINT('',(7.6,5.7,29.8));
#22246=CARTESIAN_POINT('',(7.2,2.95,29.8));
#22247=CARTESIAN_POINT('',(4.4,8.,31.5));
#22248=CARTESIAN_POINT('',(7.6,8.,31.5));
#22249=CARTESIAN_POINT('',(-2.9,-2.9,0.8));
#22250=CARTESIAN_POINT('',(-2.9,2.9,0.8));
#22251=CARTESIAN_POINT('',(2.9,-2.9,0.8));
#22252=CARTESIAN_POINT('',(2.9,2.9,0.8));
#22253=CARTESIAN_POINT('',(-1.8,-1.8,0.));
#22254=CARTESIAN_POINT('',(-1.8,1.8,0.));
#22255=CARTESIAN_POINT('',(1.8,-1.8,0.));
#22256=CARTESIAN_POINT('',(1.8,1.8,0.));
#22257=CARTESIAN_POINT('',(0.,-6.,-1.2));
#22258=CARTESIAN_POINT('',(0.,-6.,31.5));
#22259=CARTESIAN_POINT('',(0.,6.,-1.2));
#22260=CARTESIAN_POINT('',(0.,6.,31.5));
#22261=CARTESIAN_POINT('',(0.,0.,0.));
#22262=CARTESIAN_POINT('',(0.,0.,0.));
#22263=CARTESIAN_POINT('',(0.,0.,0.));
#22264=CARTESIAN_POINT('',(0.,0.,0.));
#22265=CARTESIAN_POINT('',(0.,0.,0.));
#22266=CARTESIAN_POINT('',(0.,0.,0.));
#22267=CARTESIAN_POINT('',(-6.,-4.,13.6));
#22268=CARTESIAN_POINT('',(-4.86862915010153,-2.86862915010152,16.3));
#22269=CARTESIAN_POINT('',(-7.13137084989848,-2.86862915010152,16.3));
#22270=CARTESIAN_POINT('',(-7.13137084989848,-5.13137084989848,16.3));
#22271=CARTESIAN_POINT('',(-4.86862915010152,-5.13137084989848,16.3));
#22272=CARTESIAN_POINT('',(-6.,4.,13.6));
#22273=CARTESIAN_POINT('',(-4.86862915010153,5.13137084989847,16.3));
#22274=CARTESIAN_POINT('',(-7.13137084989848,5.13137084989848,16.3));
#22275=CARTESIAN_POINT('',(-7.13137084989848,2.86862915010152,16.3));
#22276=CARTESIAN_POINT('',(-4.86862915010152,2.86862915010152,16.3));
#22277=CARTESIAN_POINT('',(6.,-4.,13.6));
#22278=CARTESIAN_POINT('',(7.13137084989848,-2.86862915010152,16.3));
#22279=CARTESIAN_POINT('',(4.86862915010152,-2.86862915010152,16.3));
#22280=CARTESIAN_POINT('',(4.86862915010152,-5.13137084989848,16.3));
#22281=CARTESIAN_POINT('',(7.13137084989847,-5.13137084989848,16.3));
#22282=CARTESIAN_POINT('',(6.,4.,13.6));
#22283=CARTESIAN_POINT('',(7.13137084989848,5.13137084989847,16.3));
#22284=CARTESIAN_POINT('',(4.86862915010153,5.13137084989848,16.3));
#22285=CARTESIAN_POINT('',(4.86862915010152,2.86862915010152,16.3));
#22286=CARTESIAN_POINT('',(7.13137084989848,2.86862915010152,16.3));
#22287=CARTESIAN_POINT('',(-1.,0.,16.3));
#22288=CARTESIAN_POINT('',(1.,0.,16.3));
#22289=CARTESIAN_POINT('',(0.,-1.,16.3));
#22290=CARTESIAN_POINT('',(-8.88178419700125E-16,1.,16.3));
#22291=CARTESIAN_POINT('',(0.,0.,0.));
#22292=CARTESIAN_POINT('',(0.,0.,0.));
#22293=UNCERTAINTY_MEASURE_WITH_UNIT(LENGTH_MEASURE(0.001),#22395,
'DISTANCE_ACCURACY_VALUE',
'Maximum model space distance between geometric entities at asserted c
onnectivities');
#22294=UNCERTAINTY_MEASURE_WITH_UNIT(LENGTH_MEASURE(0.001),#22395,
'DISTANCE_ACCURACY_VALUE',
'Maximum model space distance between geometric entities at asserted c
onnectivities');
#22295=UNCERTAINTY_MEASURE_WITH_UNIT(LENGTH_MEASURE(0.001),#22395,
'DISTANCE_ACCURACY_VALUE',
'Maximum model space distance between geometric entities at asserted c
onnectivities');
#22296=UNCERTAINTY_MEASURE_WITH_UNIT(LENGTH_MEASURE(0.001),#22395,
'DISTANCE_ACCURACY_VALUE',
'Maximum model space distance between geometric entities at asserted c
onnectivities');
#22297=UNCERTAINTY_MEASURE_WITH_UNIT(LENGTH_MEASURE(0.001),#22395,
'DISTANCE_ACCURACY_VALUE',
'Maximum model space distance between geometric entities at asserted c
onnectivities');
#22298=UNCERTAINTY_MEASURE_WITH_UNIT(LENGTH_MEASURE(0.001),#22395,
'DISTANCE_ACCURACY_VALUE',
'Maximum model space distance between geometric entities at asserted c
onnectivities');
#22299=UNCERTAINTY_MEASURE_WITH_UNIT(LENGTH_MEASURE(0.001),#22395,
'DISTANCE_ACCURACY_VALUE',
'Maximum model space distance between geometric entities at asserted c
onnectivities');
#22300=UNCERTAINTY_MEASURE_WITH_UNIT(LENGTH_MEASURE(0.001),#22395,
'DISTANCE_ACCURACY_VALUE',
'Maximum model space distance between geometric entities at asserted c
onnectivities');
#22301=UNCERTAINTY_MEASURE_WITH_UNIT(LENGTH_MEASURE(0.001),#22395,
'DISTANCE_ACCURACY_VALUE',
'Maximum model space distance between geometric entities at asserted c
onnectivities');
#22302=UNCERTAINTY_MEASURE_WITH_UNIT(LENGTH_MEASURE(0.001),#22395,
'DISTANCE_ACCURACY_VALUE',
'Maximum model space distance between geometric entities at asserted c
onnectivities');
#22303=UNCERTAINTY_MEASURE_WITH_UNIT(LENGTH_MEASURE(0.001),#22395,
'DISTANCE_ACCURACY_VALUE',
'Maximum model space distance between geometric entities at asserted c
onnectivities');
#22304=UNCERTAINTY_MEASURE_WITH_UNIT(LENGTH_MEASURE(0.001),#22395,
'DISTANCE_ACCURACY_VALUE',
'Maximum model space distance between geometric entities at asserted c
onnectivities');
#22305=UNCERTAINTY_MEASURE_WITH_UNIT(LENGTH_MEASURE(0.001),#22395,
'DISTANCE_ACCURACY_VALUE',
'Maximum model space distance between geometric entities at asserted c
onnectivities');
#22306=UNCERTAINTY_MEASURE_WITH_UNIT(LENGTH_MEASURE(0.001),#22395,
'DISTANCE_ACCURACY_VALUE',
'Maximum model space distance between geometric entities at asserted c
onnectivities');
#22307=UNCERTAINTY_MEASURE_WITH_UNIT(LENGTH_MEASURE(0.001),#22395,
'DISTANCE_ACCURACY_VALUE',
'Maximum model space distance between geometric entities at asserted c
onnectivities');
#22308=UNCERTAINTY_MEASURE_WITH_UNIT(LENGTH_MEASURE(0.001),#22395,
'DISTANCE_ACCURACY_VALUE',
'Maximum model space distance between geometric entities at asserted c
onnectivities');
#22309=UNCERTAINTY_MEASURE_WITH_UNIT(LENGTH_MEASURE(0.001),#22395,
'DISTANCE_ACCURACY_VALUE',
'Maximum model space distance between geometric entities at asserted c
onnectivities');
#22310=UNCERTAINTY_MEASURE_WITH_UNIT(LENGTH_MEASURE(0.001),#22395,
'DISTANCE_ACCURACY_VALUE',
'Maximum model space distance between geometric entities at asserted c
onnectivities');
#22311=UNCERTAINTY_MEASURE_WITH_UNIT(LENGTH_MEASURE(0.001),#22395,
'DISTANCE_ACCURACY_VALUE',
'Maximum model space distance between geometric entities at asserted c
onnectivities');
#22312=UNCERTAINTY_MEASURE_WITH_UNIT(LENGTH_MEASURE(0.001),#22395,
'DISTANCE_ACCURACY_VALUE',
'Maximum model space distance between geometric entities at asserted c
onnectivities');
#22313=UNCERTAINTY_MEASURE_WITH_UNIT(LENGTH_MEASURE(0.001),#22395,
'DISTANCE_ACCURACY_VALUE',
'Maximum model space distance between geometric entities at asserted c
onnectivities');
#22314=UNCERTAINTY_MEASURE_WITH_UNIT(LENGTH_MEASURE(0.001),#22395,
'DISTANCE_ACCURACY_VALUE',
'Maximum model space distance between geometric entities at asserted c
onnectivities');
#22315=UNCERTAINTY_MEASURE_WITH_UNIT(LENGTH_MEASURE(0.001),#22395,
'DISTANCE_ACCURACY_VALUE',
'Maximum model space distance between geometric entities at asserted c
onnectivities');
#22316=UNCERTAINTY_MEASURE_WITH_UNIT(LENGTH_MEASURE(0.001),#22395,
'DISTANCE_ACCURACY_VALUE',
'Maximum model space distance between geometric entities at asserted c
onnectivities');
#22317=UNCERTAINTY_MEASURE_WITH_UNIT(LENGTH_MEASURE(0.001),#22395,
'DISTANCE_ACCURACY_VALUE',
'Maximum model space distance between geometric entities at asserted c
onnectivities');
#22318=UNCERTAINTY_MEASURE_WITH_UNIT(LENGTH_MEASURE(0.001),#22395,
'DISTANCE_ACCURACY_VALUE',
'Maximum model space distance between geometric entities at asserted c
onnectivities');
#22319=UNCERTAINTY_MEASURE_WITH_UNIT(LENGTH_MEASURE(0.001),#22395,
'DISTANCE_ACCURACY_VALUE',
'Maximum model space distance between geometric entities at asserted c
onnectivities');
#22320=UNCERTAINTY_MEASURE_WITH_UNIT(LENGTH_MEASURE(0.001),#22395,
'DISTANCE_ACCURACY_VALUE',
'Maximum model space distance between geometric entities at asserted c
onnectivities');
#22321=UNCERTAINTY_MEASURE_WITH_UNIT(LENGTH_MEASURE(0.001),#22395,
'DISTANCE_ACCURACY_VALUE',
'Maximum model space distance between geometric entities at asserted c
onnectivities');
#22322=UNCERTAINTY_MEASURE_WITH_UNIT(LENGTH_MEASURE(0.001),#22395,
'DISTANCE_ACCURACY_VALUE',
'Maximum model space distance between geometric entities at asserted c
onnectivities');
#22323=UNCERTAINTY_MEASURE_WITH_UNIT(LENGTH_MEASURE(0.001),#22395,
'DISTANCE_ACCURACY_VALUE',
'Maximum model space distance between geometric entities at asserted c
onnectivities');
#22324=UNCERTAINTY_MEASURE_WITH_UNIT(LENGTH_MEASURE(0.001),#22395,
'DISTANCE_ACCURACY_VALUE',
'Maximum model space distance between geometric entities at asserted c
onnectivities');
#22325=UNCERTAINTY_MEASURE_WITH_UNIT(LENGTH_MEASURE(0.001),#22395,
'DISTANCE_ACCURACY_VALUE',
'Maximum model space distance between geometric entities at asserted c
onnectivities');
#22326=UNCERTAINTY_MEASURE_WITH_UNIT(LENGTH_MEASURE(0.001),#22395,
'DISTANCE_ACCURACY_VALUE',
'Maximum model space distance between geometric entities at asserted c
onnectivities');
#22327=UNCERTAINTY_MEASURE_WITH_UNIT(LENGTH_MEASURE(0.001),#22395,
'DISTANCE_ACCURACY_VALUE',
'Maximum model space distance between geometric entities at asserted c
onnectivities');
#22328=UNCERTAINTY_MEASURE_WITH_UNIT(LENGTH_MEASURE(0.001),#22395,
'DISTANCE_ACCURACY_VALUE',
'Maximum model space distance between geometric entities at asserted c
onnectivities');
#22329=UNCERTAINTY_MEASURE_WITH_UNIT(LENGTH_MEASURE(0.001),#22395,
'DISTANCE_ACCURACY_VALUE',
'Maximum model space distance between geometric entities at asserted c
onnectivities');
#22330=UNCERTAINTY_MEASURE_WITH_UNIT(LENGTH_MEASURE(0.001),#22395,
'DISTANCE_ACCURACY_VALUE',
'Maximum model space distance between geometric entities at asserted c
onnectivities');
#22331=UNCERTAINTY_MEASURE_WITH_UNIT(LENGTH_MEASURE(0.001),#22395,
'DISTANCE_ACCURACY_VALUE',
'Maximum model space distance between geometric entities at asserted c
onnectivities');
#22332=UNCERTAINTY_MEASURE_WITH_UNIT(LENGTH_MEASURE(0.001),#22395,
'DISTANCE_ACCURACY_VALUE',
'Maximum model space distance between geometric entities at asserted c
onnectivities');
#22333=UNCERTAINTY_MEASURE_WITH_UNIT(LENGTH_MEASURE(0.001),#22395,
'DISTANCE_ACCURACY_VALUE',
'Maximum model space distance between geometric entities at asserted c
onnectivities');
#22334=UNCERTAINTY_MEASURE_WITH_UNIT(LENGTH_MEASURE(0.001),#22395,
'DISTANCE_ACCURACY_VALUE',
'Maximum model space distance between geometric entities at asserted c
onnectivities');
#22335=UNCERTAINTY_MEASURE_WITH_UNIT(LENGTH_MEASURE(0.001),#22395,
'DISTANCE_ACCURACY_VALUE',
'Maximum model space distance between geometric entities at asserted c
onnectivities');
#22336=UNCERTAINTY_MEASURE_WITH_UNIT(LENGTH_MEASURE(0.001),#22395,
'DISTANCE_ACCURACY_VALUE',
'Maximum model space distance between geometric entities at asserted c
onnectivities');
#22337=UNCERTAINTY_MEASURE_WITH_UNIT(LENGTH_MEASURE(0.001),#22395,
'DISTANCE_ACCURACY_VALUE',
'Maximum model space distance between geometric entities at asserted c
onnectivities');
#22338=UNCERTAINTY_MEASURE_WITH_UNIT(LENGTH_MEASURE(0.001),#22395,
'DISTANCE_ACCURACY_VALUE',
'Maximum model space distance between geometric entities at asserted c
onnectivities');
#22339=UNCERTAINTY_MEASURE_WITH_UNIT(LENGTH_MEASURE(0.001),#22395,
'DISTANCE_ACCURACY_VALUE',
'Maximum model space distance between geometric entities at asserted c
onnectivities');
#22340=UNCERTAINTY_MEASURE_WITH_UNIT(LENGTH_MEASURE(0.001),#22395,
'DISTANCE_ACCURACY_VALUE',
'Maximum model space distance between geometric entities at asserted c
onnectivities');
#22341=UNCERTAINTY_MEASURE_WITH_UNIT(LENGTH_MEASURE(0.001),#22395,
'DISTANCE_ACCURACY_VALUE',
'Maximum model space distance between geometric entities at asserted c
onnectivities');
#22342=UNCERTAINTY_MEASURE_WITH_UNIT(LENGTH_MEASURE(0.001),#22395,
'DISTANCE_ACCURACY_VALUE',
'Maximum model space distance between geometric entities at asserted c
onnectivities');
#22343=UNCERTAINTY_MEASURE_WITH_UNIT(LENGTH_MEASURE(0.001),#22395,
'DISTANCE_ACCURACY_VALUE',
'Maximum model space distance between geometric entities at asserted c
onnectivities');
#22344=(
GEOMETRIC_REPRESENTATION_CONTEXT(3)
GLOBAL_UNCERTAINTY_ASSIGNED_CONTEXT((#22293))
GLOBAL_UNIT_ASSIGNED_CONTEXT((#22395,#22397,#22398))
REPRESENTATION_CONTEXT('','3D')
);
#22345=(
GEOMETRIC_REPRESENTATION_CONTEXT(3)
GLOBAL_UNCERTAINTY_ASSIGNED_CONTEXT((#22294))
GLOBAL_UNIT_ASSIGNED_CONTEXT((#22395,#22397,#22398))
REPRESENTATION_CONTEXT('','3D')
);
#22346=(
GEOMETRIC_REPRESENTATION_CONTEXT(3)
GLOBAL_UNCERTAINTY_ASSIGNED_CONTEXT((#22295))
GLOBAL_UNIT_ASSIGNED_CONTEXT((#22395,#22397,#22398))
REPRESENTATION_CONTEXT('','3D')
);
#22347=(
GEOMETRIC_REPRESENTATION_CONTEXT(3)
GLOBAL_UNCERTAINTY_ASSIGNED_CONTEXT((#22296))
GLOBAL_UNIT_ASSIGNED_CONTEXT((#22395,#22397,#22398))
REPRESENTATION_CONTEXT('','3D')
);
#22348=(
GEOMETRIC_REPRESENTATION_CONTEXT(3)
GLOBAL_UNCERTAINTY_ASSIGNED_CONTEXT((#22297))
GLOBAL_UNIT_ASSIGNED_CONTEXT((#22395,#22397,#22398))
REPRESENTATION_CONTEXT('','3D')
);
#22349=(
GEOMETRIC_REPRESENTATION_CONTEXT(3)
GLOBAL_UNCERTAINTY_ASSIGNED_CONTEXT((#22298))
GLOBAL_UNIT_ASSIGNED_CONTEXT((#22395,#22397,#22398))
REPRESENTATION_CONTEXT('','3D')
);
#22350=(
GEOMETRIC_REPRESENTATION_CONTEXT(3)
GLOBAL_UNCERTAINTY_ASSIGNED_CONTEXT((#22299))
GLOBAL_UNIT_ASSIGNED_CONTEXT((#22395,#22397,#22398))
REPRESENTATION_CONTEXT('','3D')
);
#22351=(
GEOMETRIC_REPRESENTATION_CONTEXT(3)
GLOBAL_UNCERTAINTY_ASSIGNED_CONTEXT((#22300))
GLOBAL_UNIT_ASSIGNED_CONTEXT((#22395,#22397,#22398))
REPRESENTATION_CONTEXT('','3D')
);
#22352=(
GEOMETRIC_REPRESENTATION_CONTEXT(3)
GLOBAL_UNCERTAINTY_ASSIGNED_CONTEXT((#22301))
GLOBAL_UNIT_ASSIGNED_CONTEXT((#22395,#22397,#22398))
REPRESENTATION_CONTEXT('','3D')
);
#22353=(
GEOMETRIC_REPRESENTATION_CONTEXT(3)
GLOBAL_UNCERTAINTY_ASSIGNED_CONTEXT((#22302))
GLOBAL_UNIT_ASSIGNED_CONTEXT((#22395,#22397,#22398))
REPRESENTATION_CONTEXT('','3D')
);
#22354=(
GEOMETRIC_REPRESENTATION_CONTEXT(3)
GLOBAL_UNCERTAINTY_ASSIGNED_CONTEXT((#22303))
GLOBAL_UNIT_ASSIGNED_CONTEXT((#22395,#22397,#22398))
REPRESENTATION_CONTEXT('','3D')
);
#22355=(
GEOMETRIC_REPRESENTATION_CONTEXT(3)
GLOBAL_UNCERTAINTY_ASSIGNED_CONTEXT((#22304))
GLOBAL_UNIT_ASSIGNED_CONTEXT((#22395,#22397,#22398))
REPRESENTATION_CONTEXT('','3D')
);
#22356=(
GEOMETRIC_REPRESENTATION_CONTEXT(3)
GLOBAL_UNCERTAINTY_ASSIGNED_CONTEXT((#22305))
GLOBAL_UNIT_ASSIGNED_CONTEXT((#22395,#22397,#22398))
REPRESENTATION_CONTEXT('','3D')
);
#22357=(
GEOMETRIC_REPRESENTATION_CONTEXT(3)
GLOBAL_UNCERTAINTY_ASSIGNED_CONTEXT((#22306))
GLOBAL_UNIT_ASSIGNED_CONTEXT((#22395,#22397,#22398))
REPRESENTATION_CONTEXT('','3D')
);
#22358=(
GEOMETRIC_REPRESENTATION_CONTEXT(3)
GLOBAL_UNCERTAINTY_ASSIGNED_CONTEXT((#22307))
GLOBAL_UNIT_ASSIGNED_CONTEXT((#22395,#22397,#22398))
REPRESENTATION_CONTEXT('','3D')
);
#22359=(
GEOMETRIC_REPRESENTATION_CONTEXT(3)
GLOBAL_UNCERTAINTY_ASSIGNED_CONTEXT((#22308))
GLOBAL_UNIT_ASSIGNED_CONTEXT((#22395,#22397,#22398))
REPRESENTATION_CONTEXT('','3D')
);
#22360=(
GEOMETRIC_REPRESENTATION_CONTEXT(3)
GLOBAL_UNCERTAINTY_ASSIGNED_CONTEXT((#22309))
GLOBAL_UNIT_ASSIGNED_CONTEXT((#22395,#22397,#22398))
REPRESENTATION_CONTEXT('','3D')
);
#22361=(
GEOMETRIC_REPRESENTATION_CONTEXT(3)
GLOBAL_UNCERTAINTY_ASSIGNED_CONTEXT((#22310))
GLOBAL_UNIT_ASSIGNED_CONTEXT((#22395,#22397,#22398))
REPRESENTATION_CONTEXT('','3D')
);
#22362=(
GEOMETRIC_REPRESENTATION_CONTEXT(3)
GLOBAL_UNCERTAINTY_ASSIGNED_CONTEXT((#22311))
GLOBAL_UNIT_ASSIGNED_CONTEXT((#22395,#22397,#22398))
REPRESENTATION_CONTEXT('','3D')
);
#22363=(
GEOMETRIC_REPRESENTATION_CONTEXT(3)
GLOBAL_UNCERTAINTY_ASSIGNED_CONTEXT((#22312))
GLOBAL_UNIT_ASSIGNED_CONTEXT((#22395,#22397,#22398))
REPRESENTATION_CONTEXT('','3D')
);
#22364=(
GEOMETRIC_REPRESENTATION_CONTEXT(3)
GLOBAL_UNCERTAINTY_ASSIGNED_CONTEXT((#22313))
GLOBAL_UNIT_ASSIGNED_CONTEXT((#22395,#22397,#22398))
REPRESENTATION_CONTEXT('','3D')
);
#22365=(
GEOMETRIC_REPRESENTATION_CONTEXT(3)
GLOBAL_UNCERTAINTY_ASSIGNED_CONTEXT((#22314))
GLOBAL_UNIT_ASSIGNED_CONTEXT((#22395,#22397,#22398))
REPRESENTATION_CONTEXT('','3D')
);
#22366=(
GEOMETRIC_REPRESENTATION_CONTEXT(3)
GLOBAL_UNCERTAINTY_ASSIGNED_CONTEXT((#22315))
GLOBAL_UNIT_ASSIGNED_CONTEXT((#22395,#22397,#22398))
REPRESENTATION_CONTEXT('','3D')
);
#22367=(
GEOMETRIC_REPRESENTATION_CONTEXT(3)
GLOBAL_UNCERTAINTY_ASSIGNED_CONTEXT((#22316))
GLOBAL_UNIT_ASSIGNED_CONTEXT((#22395,#22397,#22398))
REPRESENTATION_CONTEXT('','3D')
);
#22368=(
GEOMETRIC_REPRESENTATION_CONTEXT(3)
GLOBAL_UNCERTAINTY_ASSIGNED_CONTEXT((#22317))
GLOBAL_UNIT_ASSIGNED_CONTEXT((#22395,#22397,#22398))
REPRESENTATION_CONTEXT('','3D')
);
#22369=(
GEOMETRIC_REPRESENTATION_CONTEXT(3)
GLOBAL_UNCERTAINTY_ASSIGNED_CONTEXT((#22318))
GLOBAL_UNIT_ASSIGNED_CONTEXT((#22395,#22397,#22398))
REPRESENTATION_CONTEXT('','3D')
);
#22370=(
GEOMETRIC_REPRESENTATION_CONTEXT(3)
GLOBAL_UNCERTAINTY_ASSIGNED_CONTEXT((#22319))
GLOBAL_UNIT_ASSIGNED_CONTEXT((#22395,#22397,#22398))
REPRESENTATION_CONTEXT('','3D')
);
#22371=(
GEOMETRIC_REPRESENTATION_CONTEXT(3)
GLOBAL_UNCERTAINTY_ASSIGNED_CONTEXT((#22320))
GLOBAL_UNIT_ASSIGNED_CONTEXT((#22395,#22397,#22398))
REPRESENTATION_CONTEXT('','3D')
);
#22372=(
GEOMETRIC_REPRESENTATION_CONTEXT(3)
GLOBAL_UNCERTAINTY_ASSIGNED_CONTEXT((#22321))
GLOBAL_UNIT_ASSIGNED_CONTEXT((#22395,#22397,#22398))
REPRESENTATION_CONTEXT('','3D')
);
#22373=(
GEOMETRIC_REPRESENTATION_CONTEXT(3)
GLOBAL_UNCERTAINTY_ASSIGNED_CONTEXT((#22322))
GLOBAL_UNIT_ASSIGNED_CONTEXT((#22395,#22397,#22398))
REPRESENTATION_CONTEXT('','3D')
);
#22374=(
GEOMETRIC_REPRESENTATION_CONTEXT(3)
GLOBAL_UNCERTAINTY_ASSIGNED_CONTEXT((#22323))
GLOBAL_UNIT_ASSIGNED_CONTEXT((#22395,#22397,#22398))
REPRESENTATION_CONTEXT('','3D')
);
#22375=(
GEOMETRIC_REPRESENTATION_CONTEXT(3)
GLOBAL_UNCERTAINTY_ASSIGNED_CONTEXT((#22324))
GLOBAL_UNIT_ASSIGNED_CONTEXT((#22395,#22397,#22398))
REPRESENTATION_CONTEXT('','3D')
);
#22376=(
GEOMETRIC_REPRESENTATION_CONTEXT(3)
GLOBAL_UNCERTAINTY_ASSIGNED_CONTEXT((#22325))
GLOBAL_UNIT_ASSIGNED_CONTEXT((#22395,#22397,#22398))
REPRESENTATION_CONTEXT('','3D')
);
#22377=(
GEOMETRIC_REPRESENTATION_CONTEXT(3)
GLOBAL_UNCERTAINTY_ASSIGNED_CONTEXT((#22326))
GLOBAL_UNIT_ASSIGNED_CONTEXT((#22395,#22397,#22398))
REPRESENTATION_CONTEXT('','3D')
);
#22378=(
GEOMETRIC_REPRESENTATION_CONTEXT(3)
GLOBAL_UNCERTAINTY_ASSIGNED_CONTEXT((#22327))
GLOBAL_UNIT_ASSIGNED_CONTEXT((#22395,#22397,#22398))
REPRESENTATION_CONTEXT('','3D')
);
#22379=(
GEOMETRIC_REPRESENTATION_CONTEXT(3)
GLOBAL_UNCERTAINTY_ASSIGNED_CONTEXT((#22328))
GLOBAL_UNIT_ASSIGNED_CONTEXT((#22395,#22397,#22398))
REPRESENTATION_CONTEXT('','3D')
);
#22380=(
GEOMETRIC_REPRESENTATION_CONTEXT(3)
GLOBAL_UNCERTAINTY_ASSIGNED_CONTEXT((#22329))
GLOBAL_UNIT_ASSIGNED_CONTEXT((#22395,#22397,#22398))
REPRESENTATION_CONTEXT('','3D')
);
#22381=(
GEOMETRIC_REPRESENTATION_CONTEXT(3)
GLOBAL_UNCERTAINTY_ASSIGNED_CONTEXT((#22330))
GLOBAL_UNIT_ASSIGNED_CONTEXT((#22395,#22397,#22398))
REPRESENTATION_CONTEXT('','3D')
);
#22382=(
GEOMETRIC_REPRESENTATION_CONTEXT(3)
GLOBAL_UNCERTAINTY_ASSIGNED_CONTEXT((#22331))
GLOBAL_UNIT_ASSIGNED_CONTEXT((#22395,#22397,#22398))
REPRESENTATION_CONTEXT('','3D')
);
#22383=(
GEOMETRIC_REPRESENTATION_CONTEXT(3)
GLOBAL_UNCERTAINTY_ASSIGNED_CONTEXT((#22332))
GLOBAL_UNIT_ASSIGNED_CONTEXT((#22395,#22397,#22398))
REPRESENTATION_CONTEXT('','3D')
);
#22384=(
GEOMETRIC_REPRESENTATION_CONTEXT(3)
GLOBAL_UNCERTAINTY_ASSIGNED_CONTEXT((#22333))
GLOBAL_UNIT_ASSIGNED_CONTEXT((#22395,#22397,#22398))
REPRESENTATION_CONTEXT('','3D')
);
#22385=(
GEOMETRIC_REPRESENTATION_CONTEXT(3)
GLOBAL_UNCERTAINTY_ASSIGNED_CONTEXT((#22334))
GLOBAL_UNIT_ASSIGNED_CONTEXT((#22395,#22397,#22398))
REPRESENTATION_CONTEXT('','3D')
);
#22386=(
GEOMETRIC_REPRESENTATION_CONTEXT(3)
GLOBAL_UNCERTAINTY_ASSIGNED_CONTEXT((#22335))
GLOBAL_UNIT_ASSIGNED_CONTEXT((#22395,#22397,#22398))
REPRESENTATION_CONTEXT('','3D')
);
#22387=(
GEOMETRIC_REPRESENTATION_CONTEXT(3)
GLOBAL_UNCERTAINTY_ASSIGNED_CONTEXT((#22336))
GLOBAL_UNIT_ASSIGNED_CONTEXT((#22395,#22397,#22398))
REPRESENTATION_CONTEXT('','3D')
);
#22388=(
GEOMETRIC_REPRESENTATION_CONTEXT(3)
GLOBAL_UNCERTAINTY_ASSIGNED_CONTEXT((#22337))
GLOBAL_UNIT_ASSIGNED_CONTEXT((#22395,#22397,#22398))
REPRESENTATION_CONTEXT('','3D')
);
#22389=(
GEOMETRIC_REPRESENTATION_CONTEXT(3)
GLOBAL_UNCERTAINTY_ASSIGNED_CONTEXT((#22338))
GLOBAL_UNIT_ASSIGNED_CONTEXT((#22395,#22397,#22398))
REPRESENTATION_CONTEXT('','3D')
);
#22390=(
GEOMETRIC_REPRESENTATION_CONTEXT(3)
GLOBAL_UNCERTAINTY_ASSIGNED_CONTEXT((#22339))
GLOBAL_UNIT_ASSIGNED_CONTEXT((#22395,#22397,#22398))
REPRESENTATION_CONTEXT('','3D')
);
#22391=(
GEOMETRIC_REPRESENTATION_CONTEXT(3)
GLOBAL_UNCERTAINTY_ASSIGNED_CONTEXT((#22340))
GLOBAL_UNIT_ASSIGNED_CONTEXT((#22395,#22397,#22398))
REPRESENTATION_CONTEXT('','3D')
);
#22392=(
GEOMETRIC_REPRESENTATION_CONTEXT(3)
GLOBAL_UNCERTAINTY_ASSIGNED_CONTEXT((#22341))
GLOBAL_UNIT_ASSIGNED_CONTEXT((#22395,#22397,#22398))
REPRESENTATION_CONTEXT('','3D')
);
#22393=(
GEOMETRIC_REPRESENTATION_CONTEXT(3)
GLOBAL_UNCERTAINTY_ASSIGNED_CONTEXT((#22342))
GLOBAL_UNIT_ASSIGNED_CONTEXT((#22395,#22397,#22398))
REPRESENTATION_CONTEXT('','3D')
);
#22394=(
GEOMETRIC_REPRESENTATION_CONTEXT(3)
GLOBAL_UNCERTAINTY_ASSIGNED_CONTEXT((#22343))
GLOBAL_UNIT_ASSIGNED_CONTEXT((#22395,#22397,#22398))
REPRESENTATION_CONTEXT('','3D')
);
#22395=(
LENGTH_UNIT()
NAMED_UNIT(*)
SI_UNIT(.CENTI.,.METRE.)
);
#22396=(
LENGTH_UNIT()
NAMED_UNIT(*)
SI_UNIT($,.METRE.)
);
#22397=(
NAMED_UNIT(*)
PLANE_ANGLE_UNIT()
SI_UNIT($,.RADIAN.)
);
#22398=(
NAMED_UNIT(*)
SI_UNIT($,.STERADIAN.)
SOLID_ANGLE_UNIT()
);
#22399=SHAPE_DEFINITION_REPRESENTATION(#22449,#22638);
#22400=SHAPE_DEFINITION_REPRESENTATION(#22450,#22639);
#22401=SHAPE_DEFINITION_REPRESENTATION(#22451,#22640);
#22402=SHAPE_DEFINITION_REPRESENTATION(#22452,#22641);
#22403=SHAPE_DEFINITION_REPRESENTATION(#22453,#22642);
#22404=SHAPE_DEFINITION_REPRESENTATION(#22454,#22643);
#22405=SHAPE_DEFINITION_REPRESENTATION(#22455,#22644);
#22406=SHAPE_DEFINITION_REPRESENTATION(#22456,#22645);
#22407=SHAPE_DEFINITION_REPRESENTATION(#22457,#22646);
#22408=SHAPE_DEFINITION_REPRESENTATION(#22458,#22647);
#22409=SHAPE_DEFINITION_REPRESENTATION(#22459,#22648);
#22410=SHAPE_DEFINITION_REPRESENTATION(#22460,#22649);
#22411=SHAPE_DEFINITION_REPRESENTATION(#22461,#22650);
#22412=SHAPE_DEFINITION_REPRESENTATION(#22462,#22651);
#22413=SHAPE_DEFINITION_REPRESENTATION(#22463,#22652);
#22414=SHAPE_DEFINITION_REPRESENTATION(#22464,#22653);
#22415=SHAPE_DEFINITION_REPRESENTATION(#22465,#22654);
#22416=SHAPE_DEFINITION_REPRESENTATION(#22466,#22655);
#22417=SHAPE_DEFINITION_REPRESENTATION(#22467,#22656);
#22418=SHAPE_DEFINITION_REPRESENTATION(#22468,#22657);
#22419=SHAPE_DEFINITION_REPRESENTATION(#22469,#22658);
#22420=SHAPE_DEFINITION_REPRESENTATION(#22470,#22659);
#22421=SHAPE_DEFINITION_REPRESENTATION(#22471,#22660);
#22422=SHAPE_DEFINITION_REPRESENTATION(#22472,#22661);
#22423=SHAPE_DEFINITION_REPRESENTATION(#22473,#22662);
#22424=SHAPE_DEFINITION_REPRESENTATION(#22474,#22663);
#22425=SHAPE_DEFINITION_REPRESENTATION(#22475,#22664);
#22426=SHAPE_DEFINITION_REPRESENTATION(#22476,#22665);
#22427=SHAPE_DEFINITION_REPRESENTATION(#22477,#22666);
#22428=SHAPE_DEFINITION_REPRESENTATION(#22478,#22667);
#22429=SHAPE_DEFINITION_REPRESENTATION(#22479,#22668);
#22430=SHAPE_DEFINITION_REPRESENTATION(#22480,#22669);
#22431=SHAPE_DEFINITION_REPRESENTATION(#22481,#22670);
#22432=SHAPE_DEFINITION_REPRESENTATION(#22482,#22671);
#22433=SHAPE_DEFINITION_REPRESENTATION(#22483,#22672);
#22434=SHAPE_DEFINITION_REPRESENTATION(#22484,#22673);
#22435=SHAPE_DEFINITION_REPRESENTATION(#22485,#22674);
#22436=SHAPE_DEFINITION_REPRESENTATION(#22486,#22675);
#22437=SHAPE_DEFINITION_REPRESENTATION(#22487,#22676);
#22438=SHAPE_DEFINITION_REPRESENTATION(#22488,#22677);
#22439=SHAPE_DEFINITION_REPRESENTATION(#22489,#22678);
#22440=SHAPE_DEFINITION_REPRESENTATION(#22490,#22679);
#22441=SHAPE_DEFINITION_REPRESENTATION(#22491,#22680);
#22442=SHAPE_DEFINITION_REPRESENTATION(#22492,#22681);
#22443=SHAPE_DEFINITION_REPRESENTATION(#22493,#22682);
#22444=SHAPE_DEFINITION_REPRESENTATION(#22494,#22683);
#22445=SHAPE_DEFINITION_REPRESENTATION(#22495,#22684);
#22446=SHAPE_DEFINITION_REPRESENTATION(#22496,#22685);
#22447=SHAPE_DEFINITION_REPRESENTATION(#22497,#22686);
#22448=SHAPE_DEFINITION_REPRESENTATION(#22500,#22687);
#22449=PRODUCT_DEFINITION_SHAPE('',$,#22689);
#22450=PRODUCT_DEFINITION_SHAPE('',$,#22690);
#22451=PRODUCT_DEFINITION_SHAPE('',$,#22691);
#22452=PRODUCT_DEFINITION_SHAPE('',$,#22692);
#22453=PRODUCT_DEFINITION_SHAPE('',$,#22693);
#22454=PRODUCT_DEFINITION_SHAPE('',$,#22694);
#22455=PRODUCT_DEFINITION_SHAPE('',$,#22695);
#22456=PRODUCT_DEFINITION_SHAPE('',$,#22696);
#22457=PRODUCT_DEFINITION_SHAPE('',$,#22697);
#22458=PRODUCT_DEFINITION_SHAPE('',$,#22698);
#22459=PRODUCT_DEFINITION_SHAPE('',$,#22699);
#22460=PRODUCT_DEFINITION_SHAPE('',$,#22700);
#22461=PRODUCT_DEFINITION_SHAPE('',$,#22701);
#22462=PRODUCT_DEFINITION_SHAPE('',$,#22702);
#22463=PRODUCT_DEFINITION_SHAPE('',$,#22703);
#22464=PRODUCT_DEFINITION_SHAPE('',$,#22704);
#22465=PRODUCT_DEFINITION_SHAPE('',$,#22705);
#22466=PRODUCT_DEFINITION_SHAPE('',$,#22706);
#22467=PRODUCT_DEFINITION_SHAPE('',$,#22707);
#22468=PRODUCT_DEFINITION_SHAPE('',$,#22708);
#22469=PRODUCT_DEFINITION_SHAPE('',$,#22709);
#22470=PRODUCT_DEFINITION_SHAPE('',$,#22710);
#22471=PRODUCT_DEFINITION_SHAPE('',$,#22711);
#22472=PRODUCT_DEFINITION_SHAPE('',$,#22712);
#22473=PRODUCT_DEFINITION_SHAPE('',$,#22713);
#22474=PRODUCT_DEFINITION_SHAPE('',$,#22714);
#22475=PRODUCT_DEFINITION_SHAPE('',$,#22715);
#22476=PRODUCT_DEFINITION_SHAPE('',$,#22716);
#22477=PRODUCT_DEFINITION_SHAPE('',$,#22717);
#22478=PRODUCT_DEFINITION_SHAPE('',$,#22718);
#22479=PRODUCT_DEFINITION_SHAPE('',$,#22719);
#22480=PRODUCT_DEFINITION_SHAPE('',$,#22720);
#22481=PRODUCT_DEFINITION_SHAPE('',$,#22721);
#22482=PRODUCT_DEFINITION_SHAPE('',$,#22722);
#22483=PRODUCT_DEFINITION_SHAPE('',$,#22723);
#22484=PRODUCT_DEFINITION_SHAPE('',$,#22724);
#22485=PRODUCT_DEFINITION_SHAPE('',$,#22725);
#22486=PRODUCT_DEFINITION_SHAPE('',$,#22726);
#22487=PRODUCT_DEFINITION_SHAPE('',$,#22727);
#22488=PRODUCT_DEFINITION_SHAPE('',$,#22728);
#22489=PRODUCT_DEFINITION_SHAPE('',$,#22729);
#22490=PRODUCT_DEFINITION_SHAPE('',$,#22730);
#22491=PRODUCT_DEFINITION_SHAPE('',$,#22731);
#22492=PRODUCT_DEFINITION_SHAPE('',$,#22732);
#22493=PRODUCT_DEFINITION_SHAPE('',$,#22733);
#22494=PRODUCT_DEFINITION_SHAPE('',$,#22734);
#22495=PRODUCT_DEFINITION_SHAPE('',$,#22735);
#22496=PRODUCT_DEFINITION_SHAPE('',$,#22736);
#22497=PRODUCT_DEFINITION_SHAPE('',$,#22737);
#22498=PRODUCT_DEFINITION_SHAPE($,$,#428);
#22499=PRODUCT_DEFINITION_SHAPE($,$,#429);
#22500=PRODUCT_DEFINITION_SHAPE('',$,#22738);
#22501=PRODUCT_DEFINITION_SHAPE($,$,#430);
#22502=PRODUCT_DEFINITION_SHAPE($,$,#431);
#22503=PRODUCT_DEFINITION_SHAPE($,$,#432);
#22504=PRODUCT_DEFINITION_SHAPE($,$,#433);
#22505=PRODUCT_DEFINITION_SHAPE($,$,#434);
#22506=PRODUCT_DEFINITION_SHAPE($,$,#435);
#22507=PRODUCT_DEFINITION_SHAPE($,$,#436);
#22508=PRODUCT_DEFINITION_SHAPE($,$,#437);
#22509=PRODUCT_DEFINITION_SHAPE($,$,#438);
#22510=PRODUCT_DEFINITION_SHAPE($,$,#439);
#22511=PRODUCT_DEFINITION_SHAPE($,$,#440);
#22512=PRODUCT_DEFINITION_SHAPE($,$,#441);
#22513=PRODUCT_DEFINITION_SHAPE($,$,#442);
#22514=PRODUCT_DEFINITION_SHAPE($,$,#443);
#22515=PRODUCT_DEFINITION_SHAPE($,$,#444);
#22516=PRODUCT_DEFINITION_SHAPE($,$,#445);
#22517=PRODUCT_DEFINITION_SHAPE($,$,#446);
#22518=PRODUCT_DEFINITION_SHAPE($,$,#447);
#22519=PRODUCT_DEFINITION_SHAPE($,$,#448);
#22520=PRODUCT_DEFINITION_SHAPE($,$,#449);
#22521=PRODUCT_DEFINITION_SHAPE($,$,#450);
#22522=PRODUCT_DEFINITION_SHAPE($,$,#451);
#22523=PRODUCT_DEFINITION_SHAPE($,$,#452);
#22524=PRODUCT_DEFINITION_SHAPE($,$,#453);
#22525=PRODUCT_DEFINITION_SHAPE($,$,#454);
#22526=PRODUCT_DEFINITION_SHAPE($,$,#455);
#22527=PRODUCT_DEFINITION_SHAPE($,$,#456);
#22528=PRODUCT_DEFINITION_SHAPE($,$,#457);
#22529=PRODUCT_DEFINITION_SHAPE($,$,#458);
#22530=PRODUCT_DEFINITION_SHAPE($,$,#459);
#22531=PRODUCT_DEFINITION_SHAPE($,$,#460);
#22532=PRODUCT_DEFINITION_SHAPE($,$,#461);
#22533=PRODUCT_DEFINITION_SHAPE($,$,#462);
#22534=PRODUCT_DEFINITION_SHAPE($,$,#463);
#22535=PRODUCT_DEFINITION_SHAPE($,$,#464);
#22536=PRODUCT_DEFINITION_SHAPE($,$,#465);
#22537=PRODUCT_DEFINITION_SHAPE($,$,#466);
#22538=PRODUCT_DEFINITION_SHAPE($,$,#467);
#22539=PRODUCT_DEFINITION_SHAPE($,$,#468);
#22540=PRODUCT_DEFINITION_SHAPE($,$,#469);
#22541=PRODUCT_DEFINITION_SHAPE($,$,#470);
#22542=PRODUCT_DEFINITION_SHAPE($,$,#471);
#22543=PRODUCT_DEFINITION_SHAPE($,$,#472);
#22544=PRODUCT_DEFINITION_SHAPE($,$,#473);
#22545=PRODUCT_DEFINITION_SHAPE($,$,#474);
#22546=PRODUCT_DEFINITION_SHAPE($,$,#475);
#22547=PRODUCT_DEFINITION_SHAPE($,$,#476);
#22548=PRODUCT_DEFINITION_SHAPE($,$,#477);
#22549=PRODUCT_DEFINITION_SHAPE($,$,#478);
#22550=PRODUCT_DEFINITION_SHAPE($,$,#479);
#22551=PRODUCT_DEFINITION_SHAPE($,$,#480);
#22552=PRODUCT_DEFINITION_SHAPE($,$,#481);
#22553=PRODUCT_DEFINITION_SHAPE($,$,#482);
#22554=PRODUCT_DEFINITION_SHAPE($,$,#483);
#22555=PRODUCT_DEFINITION_SHAPE($,$,#484);
#22556=PRODUCT_DEFINITION_SHAPE($,$,#485);
#22557=PRODUCT_DEFINITION_SHAPE($,$,#486);
#22558=PRODUCT_DEFINITION_SHAPE($,$,#487);
#22559=PRODUCT_DEFINITION_SHAPE($,$,#488);
#22560=PRODUCT_DEFINITION_SHAPE($,$,#489);
#22561=PRODUCT_DEFINITION_SHAPE($,$,#490);
#22562=PRODUCT_DEFINITION_SHAPE($,$,#491);
#22563=PRODUCT_DEFINITION_SHAPE($,$,#492);
#22564=PRODUCT_DEFINITION_SHAPE($,$,#493);
#22565=PRODUCT_DEFINITION_SHAPE($,$,#494);
#22566=PRODUCT_DEFINITION_SHAPE($,$,#495);
#22567=PRODUCT_DEFINITION_SHAPE($,$,#496);
#22568=PRODUCT_DEFINITION_SHAPE($,$,#497);
#22569=PRODUCT_DEFINITION_SHAPE($,$,#498);
#22570=PRODUCT_DEFINITION_SHAPE($,$,#499);
#22571=PRODUCT_DEFINITION_SHAPE($,$,#500);
#22572=PRODUCT_DEFINITION_SHAPE($,$,#501);
#22573=PRODUCT_DEFINITION_SHAPE($,$,#502);
#22574=PRODUCT_DEFINITION_SHAPE($,$,#503);
#22575=PRODUCT_DEFINITION_SHAPE($,$,#504);
#22576=PRODUCT_DEFINITION_SHAPE($,$,#505);
#22577=PRODUCT_DEFINITION_SHAPE($,$,#506);
#22578=PRODUCT_DEFINITION_SHAPE($,$,#507);
#22579=PRODUCT_DEFINITION_SHAPE($,$,#508);
#22580=PRODUCT_DEFINITION_SHAPE($,$,#509);
#22581=PRODUCT_DEFINITION_SHAPE($,$,#510);
#22582=PRODUCT_DEFINITION_SHAPE($,$,#511);
#22583=PRODUCT_DEFINITION_SHAPE($,$,#512);
#22584=PRODUCT_DEFINITION_SHAPE($,$,#513);
#22585=PRODUCT_DEFINITION_SHAPE($,$,#514);
#22586=PRODUCT_DEFINITION_SHAPE($,$,#515);
#22587=PRODUCT_DEFINITION_SHAPE($,$,#516);
#22588=PRODUCT_DEFINITION_SHAPE($,$,#517);
#22589=PRODUCT_DEFINITION_SHAPE($,$,#518);
#22590=PRODUCT_DEFINITION_SHAPE($,$,#519);
#22591=PRODUCT_DEFINITION_SHAPE($,$,#520);
#22592=PRODUCT_DEFINITION_SHAPE($,$,#521);
#22593=PRODUCT_DEFINITION_SHAPE($,$,#522);
#22594=PRODUCT_DEFINITION_SHAPE($,$,#523);
#22595=PRODUCT_DEFINITION_SHAPE($,$,#524);
#22596=PRODUCT_DEFINITION_SHAPE($,$,#525);
#22597=PRODUCT_DEFINITION_SHAPE($,$,#526);
#22598=PRODUCT_DEFINITION_SHAPE($,$,#527);
#22599=PRODUCT_DEFINITION_SHAPE($,$,#528);
#22600=PRODUCT_DEFINITION_SHAPE($,$,#529);
#22601=PRODUCT_DEFINITION_SHAPE($,$,#530);
#22602=PRODUCT_DEFINITION_SHAPE($,$,#531);
#22603=PRODUCT_DEFINITION_SHAPE($,$,#532);
#22604=PRODUCT_DEFINITION_SHAPE($,$,#533);
#22605=PRODUCT_DEFINITION_SHAPE($,$,#534);
#22606=PRODUCT_DEFINITION_SHAPE($,$,#535);
#22607=PRODUCT_DEFINITION_SHAPE($,$,#536);
#22608=PRODUCT_DEFINITION_SHAPE($,$,#537);
#22609=PRODUCT_DEFINITION_SHAPE($,$,#538);
#22610=PRODUCT_DEFINITION_SHAPE($,$,#539);
#22611=PRODUCT_DEFINITION_SHAPE($,$,#540);
#22612=PRODUCT_DEFINITION_SHAPE($,$,#541);
#22613=PRODUCT_DEFINITION_SHAPE($,$,#542);
#22614=PRODUCT_DEFINITION_SHAPE($,$,#543);
#22615=PRODUCT_DEFINITION_SHAPE($,$,#544);
#22616=PRODUCT_DEFINITION_SHAPE($,$,#545);
#22617=PRODUCT_DEFINITION_SHAPE($,$,#546);
#22618=PRODUCT_DEFINITION_SHAPE($,$,#547);
#22619=PRODUCT_DEFINITION_SHAPE($,$,#548);
#22620=PRODUCT_DEFINITION_SHAPE($,$,#549);
#22621=PRODUCT_DEFINITION_SHAPE($,$,#550);
#22622=PRODUCT_DEFINITION_SHAPE($,$,#551);
#22623=PRODUCT_DEFINITION_SHAPE($,$,#552);
#22624=PRODUCT_DEFINITION_SHAPE($,$,#553);
#22625=PRODUCT_DEFINITION_SHAPE($,$,#554);
#22626=PRODUCT_DEFINITION_SHAPE($,$,#555);
#22627=PRODUCT_DEFINITION_SHAPE($,$,#556);
#22628=PRODUCT_DEFINITION_SHAPE($,$,#557);
#22629=PRODUCT_DEFINITION_SHAPE($,$,#558);
#22630=PRODUCT_DEFINITION_SHAPE($,$,#559);
#22631=PRODUCT_DEFINITION_SHAPE($,$,#560);
#22632=PRODUCT_DEFINITION_SHAPE($,$,#561);
#22633=PRODUCT_DEFINITION_SHAPE($,$,#562);
#22634=PRODUCT_DEFINITION_SHAPE($,$,#563);
#22635=PRODUCT_DEFINITION_SHAPE($,$,#564);
#22636=PRODUCT_DEFINITION_SHAPE($,$,#565);
#22637=PRODUCT_DEFINITION_SHAPE($,$,#566);
#22638=SHAPE_REPRESENTATION('',(#9760,#10948,#10949),#22344);
#22639=SHAPE_REPRESENTATION('',(#9761,#10813,#10814,#10815,#10816,#10817,
#10818,#10819,#10820,#10821,#10822,#10823,#10824,#10825,#10826,#10827,#10828,
#10829,#10830,#10831,#10832,#10833,#10834,#10835,#10836,#10837,#10838,#10839,
#10840,#10841,#10842,#10843,#10844,#10845,#10846,#10847,#10848,#10849,#10850,
#10851,#10852,#10853,#10854,#10855,#10856,#10857,#10858,#10859,#10860,#10861,
#10862,#10863,#10864,#10865,#10866,#10867,#10868,#10869,#10870,#10871,#10872,
#10873,#10874,#10875,#10876,#10877,#10878,#10879,#10880,#10881,#10882,#10883,
#10884,#10885,#10886,#10887,#10888,#10889,#10890,#10891,#10892,#10893,#10894,
#10895,#10896,#10897,#10898,#10899,#10900,#10901,#10902,#10903,#10904,#10905,
#10906,#10907,#10908,#10909,#10910,#10911,#10912,#10913,#10914,#10915,#10916,
#10917),#22345);
#22640=SHAPE_REPRESENTATION('',(#9762),#22346);
#22641=SHAPE_REPRESENTATION('',(#9835),#22347);
#22642=SHAPE_REPRESENTATION('',(#9842),#22348);
#22643=SHAPE_REPRESENTATION('',(#9849),#22349);
#22644=SHAPE_REPRESENTATION('',(#9910),#22350);
#22645=SHAPE_REPRESENTATION('',(#9933),#22351);
#22646=SHAPE_REPRESENTATION('',(#9956),#22352);
#22647=SHAPE_REPRESENTATION('',(#9977),#22353);
#22648=SHAPE_REPRESENTATION('',(#10004),#22354);
#22649=SHAPE_REPRESENTATION('',(#10013),#22355);
#22650=SHAPE_REPRESENTATION('',(#10018),#22356);
#22651=SHAPE_REPRESENTATION('',(#10039),#22357);
#22652=SHAPE_REPRESENTATION('',(#10066),#22358);
#22653=SHAPE_REPRESENTATION('',(#10075),#22359);
#22654=SHAPE_REPRESENTATION('',(#10080),#22360);
#22655=SHAPE_REPRESENTATION('',(#10101),#22361);
#22656=SHAPE_REPRESENTATION('',(#10128),#22362);
#22657=SHAPE_REPRESENTATION('',(#10137),#22363);
#22658=SHAPE_REPRESENTATION('',(#10142),#22364);
#22659=SHAPE_REPRESENTATION('',(#10163),#22365);
#22660=SHAPE_REPRESENTATION('',(#10190),#22366);
#22661=SHAPE_REPRESENTATION('',(#10199),#22367);
#22662=SHAPE_REPRESENTATION('',(#10204),#22368);
#22663=SHAPE_REPRESENTATION('',(#10235),#22369);
#22664=SHAPE_REPRESENTATION('',(#10266),#22370);
#22665=SHAPE_REPRESENTATION('',(#10275),#22371);
#22666=SHAPE_REPRESENTATION('',(#10285),#22372);
#22667=SHAPE_REPRESENTATION('',(#10291),#22373);
#22668=SHAPE_REPRESENTATION('',(#10301),#22374);
#22669=SHAPE_REPRESENTATION('',(#10307),#22375);
#22670=SHAPE_REPRESENTATION('',(#10317),#22376);
#22671=SHAPE_REPRESENTATION('',(#10323),#22377);
#22672=SHAPE_REPRESENTATION('',(#10333),#22378);
#22673=SHAPE_REPRESENTATION('',(#10339),#22379);
#22674=SHAPE_REPRESENTATION('',(#10349),#22380);
#22675=SHAPE_REPRESENTATION('',(#10387),#22381);
#22676=SHAPE_REPRESENTATION('',(#10411),#22382);
#22677=SHAPE_REPRESENTATION('',(#10437,#10918,#10919,#10920,#10921,#10922,
#10923,#10924,#10925,#10926,#10927,#10928,#10929,#10930,#10931,#10932,#10933,
#10934,#10935,#10936,#10937,#10938,#10939,#10940,#10941,#10942,#10943,#10944,
#10945,#10946,#10947),#22383);
#22678=SHAPE_REPRESENTATION('',(#10438),#22384);
#22679=SHAPE_REPRESENTATION('',(#10517),#22385);
#22680=SHAPE_REPRESENTATION('',(#10566),#22386);
#22681=SHAPE_REPRESENTATION('',(#10615),#22387);
#22682=SHAPE_REPRESENTATION('',(#10664),#22388);
#22683=SHAPE_REPRESENTATION('',(#10713),#22389);
#22684=SHAPE_REPRESENTATION('',(#10735,#10785,#10786),#22390);
#22685=SHAPE_REPRESENTATION('',(#10736),#22391);
#22686=SHAPE_REPRESENTATION('',(#10768),#22392);
#22687=SHAPE_REPRESENTATION('',(#10787),#22393);
#22688=PRODUCT_DEFINITION_CONTEXT('part definition',#22840,'design');
#22689=PRODUCT_DEFINITION('PAT-120','PAT-120',#22739,
#22688);
#22690=PRODUCT_DEFINITION('Frame and installed return springs',
'Frame and installed return springs',#22740,#22688);
#22691=PRODUCT_DEFINITION('Base','Base',#22741,#22688);
#22692=PRODUCT_DEFINITION('Foot strip','Foot strip',#22742,#22688);
#22693=PRODUCT_DEFINITION('Foot strip (1)','Foot strip (1)',#22743,#22688);
#22694=PRODUCT_DEFINITION('Guide header','Guide header',#22744,#22688);
#22695=PRODUCT_DEFINITION('Frame upright','Frame upright',#22745,#22688);
#22696=PRODUCT_DEFINITION('Frame upright (1)','Frame upright (1)',#22746,
#22688);
#22697=PRODUCT_DEFINITION('Lower guide bracket','Lower guide bracket',#22747,
#22688);
#22698=PRODUCT_DEFINITION('Upper guide bracket','Upper guide bracket',#22748,
#22688);
#22699=PRODUCT_DEFINITION('Lower spring seat','Lower spring seat',#22749,
#22688);
#22700=PRODUCT_DEFINITION('Installed compression spring',
'Installed compression spring',#22750,#22688);
#22701=PRODUCT_DEFINITION('Lower guide bracket (1)',
'Lower guide bracket (1)',#22751,#22688);
#22702=PRODUCT_DEFINITION('Upper guide bracket (1)',
'Upper guide bracket (1)',#22752,#22688);
#22703=PRODUCT_DEFINITION('Lower spring seat (1)','Lower spring seat (1)',
#22753,#22688);
#22704=PRODUCT_DEFINITION('Installed compression spring (1)',
'Installed compression spring (1)',#22754,#22688);
#22705=PRODUCT_DEFINITION('Lower guide bracket (2)',
'Lower guide bracket (2)',#22755,#22688);
#22706=PRODUCT_DEFINITION('Upper guide bracket (2)',
'Upper guide bracket (2)',#22756,#22688);
#22707=PRODUCT_DEFINITION('Lower spring seat (2)','Lower spring seat (2)',
#22757,#22688);
#22708=PRODUCT_DEFINITION('Installed compression spring (2)',
'Installed compression spring (2)',#22758,#22688);
#22709=PRODUCT_DEFINITION('Lower guide bracket (3)',
'Lower guide bracket (3)',#22759,#22688);
#22710=PRODUCT_DEFINITION('Upper guide bracket (3)',
'Upper guide bracket (3)',#22760,#22688);
#22711=PRODUCT_DEFINITION('Lower spring seat (3)','Lower spring seat (3)',
#22761,#22688);
#22712=PRODUCT_DEFINITION('Installed compression spring (3)',
'Installed compression spring (3)',#22762,#22688);
#22713=PRODUCT_DEFINITION('Exciter envelope','Exciter envelope',#22763,
#22688);
#22714=PRODUCT_DEFINITION('Exciter base flange','Exciter base flange',#22764,
#22688);
#22715=PRODUCT_DEFINITION('Armature guide bush','Armature guide bush',#22765,
#22688);
#22716=PRODUCT_DEFINITION('Lower stop post','Lower stop post',#22766,#22688);
#22717=PRODUCT_DEFINITION('Stop bumper','Stop bumper',#22767,#22688);
#22718=PRODUCT_DEFINITION('Upper stop post','Upper stop post',#22768,#22688);
#22719=PRODUCT_DEFINITION('Stop bumper (1)','Stop bumper (1)',#22769,#22688);
#22720=PRODUCT_DEFINITION('Lower stop post (1)','Lower stop post (1)',#22770,
#22688);
#22721=PRODUCT_DEFINITION('Stop bumper (2)','Stop bumper (2)',#22771,#22688);
#22722=PRODUCT_DEFINITION('Upper stop post (1)','Upper stop post (1)',#22772,
#22688);
#22723=PRODUCT_DEFINITION('Stop bumper (3)','Stop bumper (3)',#22773,#22688);
#22724=PRODUCT_DEFINITION(
'Precision Shaft - 12 mm Diameter, 300 mm Long',
'Precision Shaft - 12 mm Diameter, 300 mm Long',#22774,#22688);
#22725=PRODUCT_DEFINITION('Shaft Support - 12 mm Bore',
'Shaft Support - 12 mm Bore',#22775,#22688);
#22726=PRODUCT_DEFINITION('M5x14 Cap Screw','M5x14 Cap Screw',#22776,#22688);
#22727=PRODUCT_DEFINITION('Cap Screw - M5x20','Cap Screw - M5x20',#22777,
#22688);
#22728=PRODUCT_DEFINITION('Guided table and armature',
'Guided table and armature',#22778,#22688);
#22729=PRODUCT_DEFINITION('Table','Table',#22779,#22688);
#22730=PRODUCT_DEFINITION('Bushing housing and upper spring seat',
'Bushing housing and upper spring seat',#22780,#22688);
#22731=PRODUCT_DEFINITION('Bushing housing and upper spring seat (1)',
'Bushing housing and upper spring seat (1)',#22781,#22688);
#22732=PRODUCT_DEFINITION('Bushing housing and upper spring seat (2)',
'Bushing housing and upper spring seat (2)',#22782,#22688);
#22733=PRODUCT_DEFINITION('Bushing housing and upper spring seat (3)',
'Bushing housing and upper spring seat (3)',#22783,#22688);
#22734=PRODUCT_DEFINITION('Armature','Armature',#22784,#22688);
#22735=PRODUCT_DEFINITION('Linear Ball Bushing - 12 x 21 x 30 mm',
'Linear Ball Bushing - 12 x 21 x 30 mm',#22785,#22688);
#22736=PRODUCT_DEFINITION('Steel sleeve','Steel sleeve',#22786,#22688);
#22737=PRODUCT_DEFINITION('Ball retainer (plastic)',
'Ball retainer (plastic)',#22787,#22688);
#22738=PRODUCT_DEFINITION('Cap Screw - M4x16','Cap Screw - M4x16',#22788,
#22688);
#22739=PRODUCT_DEFINITION_FORMATION('',$,#22842);
#22740=PRODUCT_DEFINITION_FORMATION('',$,#22843);
#22741=PRODUCT_DEFINITION_FORMATION('',$,#22844);
#22742=PRODUCT_DEFINITION_FORMATION('',$,#22845);
#22743=PRODUCT_DEFINITION_FORMATION('',$,#22846);
#22744=PRODUCT_DEFINITION_FORMATION('',$,#22847);
#22745=PRODUCT_DEFINITION_FORMATION('',$,#22848);
#22746=PRODUCT_DEFINITION_FORMATION('',$,#22849);
#22747=PRODUCT_DEFINITION_FORMATION('',$,#22850);
#22748=PRODUCT_DEFINITION_FORMATION('',$,#22851);
#22749=PRODUCT_DEFINITION_FORMATION('',$,#22852);
#22750=PRODUCT_DEFINITION_FORMATION('',$,#22853);
#22751=PRODUCT_DEFINITION_FORMATION('',$,#22854);
#22752=PRODUCT_DEFINITION_FORMATION('',$,#22855);
#22753=PRODUCT_DEFINITION_FORMATION('',$,#22856);
#22754=PRODUCT_DEFINITION_FORMATION('',$,#22857);
#22755=PRODUCT_DEFINITION_FORMATION('',$,#22858);
#22756=PRODUCT_DEFINITION_FORMATION('',$,#22859);
#22757=PRODUCT_DEFINITION_FORMATION('',$,#22860);
#22758=PRODUCT_DEFINITION_FORMATION('',$,#22861);
#22759=PRODUCT_DEFINITION_FORMATION('',$,#22862);
#22760=PRODUCT_DEFINITION_FORMATION('',$,#22863);
#22761=PRODUCT_DEFINITION_FORMATION('',$,#22864);
#22762=PRODUCT_DEFINITION_FORMATION('',$,#22865);
#22763=PRODUCT_DEFINITION_FORMATION('',$,#22866);
#22764=PRODUCT_DEFINITION_FORMATION('',$,#22867);
#22765=PRODUCT_DEFINITION_FORMATION('',$,#22868);
#22766=PRODUCT_DEFINITION_FORMATION('',$,#22869);
#22767=PRODUCT_DEFINITION_FORMATION('',$,#22870);
#22768=PRODUCT_DEFINITION_FORMATION('',$,#22871);
#22769=PRODUCT_DEFINITION_FORMATION('',$,#22872);
#22770=PRODUCT_DEFINITION_FORMATION('',$,#22873);
#22771=PRODUCT_DEFINITION_FORMATION('',$,#22874);
#22772=PRODUCT_DEFINITION_FORMATION('',$,#22875);
#22773=PRODUCT_DEFINITION_FORMATION('',$,#22876);
#22774=PRODUCT_DEFINITION_FORMATION('',$,#22877);
#22775=PRODUCT_DEFINITION_FORMATION('',$,#22878);
#22776=PRODUCT_DEFINITION_FORMATION('',$,#22879);
#22777=PRODUCT_DEFINITION_FORMATION('',$,#22880);
#22778=PRODUCT_DEFINITION_FORMATION('',$,#22881);
#22779=PRODUCT_DEFINITION_FORMATION('',$,#22882);
#22780=PRODUCT_DEFINITION_FORMATION('',$,#22883);
#22781=PRODUCT_DEFINITION_FORMATION('',$,#22884);
#22782=PRODUCT_DEFINITION_FORMATION('',$,#22885);
#22783=PRODUCT_DEFINITION_FORMATION('',$,#22886);
#22784=PRODUCT_DEFINITION_FORMATION('',$,#22887);
#22785=PRODUCT_DEFINITION_FORMATION('',$,#22888);
#22786=PRODUCT_DEFINITION_FORMATION('',$,#22889);
#22787=PRODUCT_DEFINITION_FORMATION('',$,#22890);
#22788=PRODUCT_DEFINITION_FORMATION('',$,#22891);
#22789=PRODUCT_RELATED_PRODUCT_CATEGORY('PAT-120','PAT-120',(#22842));
#22790=PRODUCT_RELATED_PRODUCT_CATEGORY(
'Frame and installed return springs',
'Frame and installed return springs',(#22843));
#22791=PRODUCT_RELATED_PRODUCT_CATEGORY('Base','Base',(#22844));
#22792=PRODUCT_RELATED_PRODUCT_CATEGORY('Foot strip','Foot strip',(#22845));
#22793=PRODUCT_RELATED_PRODUCT_CATEGORY('Foot strip (1)',
'Foot strip (1)',(#22846));
#22794=PRODUCT_RELATED_PRODUCT_CATEGORY('Guide header','Guide header',(#22847));
#22795=PRODUCT_RELATED_PRODUCT_CATEGORY('Frame upright','Frame upright',
(#22848));
#22796=PRODUCT_RELATED_PRODUCT_CATEGORY('Frame upright (1)',
'Frame upright (1)',(#22849));
#22797=PRODUCT_RELATED_PRODUCT_CATEGORY('Lower guide bracket',
'Lower guide bracket',(#22850));
#22798=PRODUCT_RELATED_PRODUCT_CATEGORY('Upper guide bracket',
'Upper guide bracket',(#22851));
#22799=PRODUCT_RELATED_PRODUCT_CATEGORY('Lower spring seat',
'Lower spring seat',(#22852));
#22800=PRODUCT_RELATED_PRODUCT_CATEGORY('Installed compression spring',
'Installed compression spring',(#22853));
#22801=PRODUCT_RELATED_PRODUCT_CATEGORY('Lower guide bracket (1)',
'Lower guide bracket (1)',(#22854));
#22802=PRODUCT_RELATED_PRODUCT_CATEGORY('Upper guide bracket (1)',
'Upper guide bracket (1)',(#22855));
#22803=PRODUCT_RELATED_PRODUCT_CATEGORY('Lower spring seat (1)',
'Lower spring seat (1)',(#22856));
#22804=PRODUCT_RELATED_PRODUCT_CATEGORY(
'Installed compression spring (1)','Installed compression spring (1)',(#22857));
#22805=PRODUCT_RELATED_PRODUCT_CATEGORY('Lower guide bracket (2)',
'Lower guide bracket (2)',(#22858));
#22806=PRODUCT_RELATED_PRODUCT_CATEGORY('Upper guide bracket (2)',
'Upper guide bracket (2)',(#22859));
#22807=PRODUCT_RELATED_PRODUCT_CATEGORY('Lower spring seat (2)',
'Lower spring seat (2)',(#22860));
#22808=PRODUCT_RELATED_PRODUCT_CATEGORY(
'Installed compression spring (2)','Installed compression spring (2)',(#22861));
#22809=PRODUCT_RELATED_PRODUCT_CATEGORY('Lower guide bracket (3)',
'Lower guide bracket (3)',(#22862));
#22810=PRODUCT_RELATED_PRODUCT_CATEGORY('Upper guide bracket (3)',
'Upper guide bracket (3)',(#22863));
#22811=PRODUCT_RELATED_PRODUCT_CATEGORY('Lower spring seat (3)',
'Lower spring seat (3)',(#22864));
#22812=PRODUCT_RELATED_PRODUCT_CATEGORY(
'Installed compression spring (3)','Installed compression spring (3)',(#22865));
#22813=PRODUCT_RELATED_PRODUCT_CATEGORY('Exciter envelope',
'Exciter envelope',(#22866));
#22814=PRODUCT_RELATED_PRODUCT_CATEGORY('Exciter base flange',
'Exciter base flange',(#22867));
#22815=PRODUCT_RELATED_PRODUCT_CATEGORY('Armature guide bush',
'Armature guide bush',(#22868));
#22816=PRODUCT_RELATED_PRODUCT_CATEGORY('Lower stop post',
'Lower stop post',(#22869));
#22817=PRODUCT_RELATED_PRODUCT_CATEGORY('Stop bumper','Stop bumper',(#22870));
#22818=PRODUCT_RELATED_PRODUCT_CATEGORY('Upper stop post',
'Upper stop post',(#22871));
#22819=PRODUCT_RELATED_PRODUCT_CATEGORY('Stop bumper (1)',
'Stop bumper (1)',(#22872));
#22820=PRODUCT_RELATED_PRODUCT_CATEGORY('Lower stop post (1)',
'Lower stop post (1)',(#22873));
#22821=PRODUCT_RELATED_PRODUCT_CATEGORY('Stop bumper (2)',
'Stop bumper (2)',(#22874));
#22822=PRODUCT_RELATED_PRODUCT_CATEGORY('Upper stop post (1)',
'Upper stop post (1)',(#22875));
#22823=PRODUCT_RELATED_PRODUCT_CATEGORY('Stop bumper (3)',
'Stop bumper (3)',(#22876));
#22824=PRODUCT_RELATED_PRODUCT_CATEGORY(
'Precision Shaft - 12 mm Diameter, 300 mm Long',
'Precision Shaft - 12 mm Diameter, 300 mm Long',(#22877));
#22825=PRODUCT_RELATED_PRODUCT_CATEGORY('Shaft Support - 12 mm Bore',
'Shaft Support - 12 mm Bore',(#22878));
#22826=PRODUCT_RELATED_PRODUCT_CATEGORY('M5x14 Cap Screw',
'M5x14 Cap Screw',(#22879));
#22827=PRODUCT_RELATED_PRODUCT_CATEGORY('Cap Screw - M5x20',
'Cap Screw - M5x20',(#22880));
#22828=PRODUCT_RELATED_PRODUCT_CATEGORY('Guided table and armature',
'Guided table and armature',(#22881));
#22829=PRODUCT_RELATED_PRODUCT_CATEGORY('Table','Table',(#22882));
#22830=PRODUCT_RELATED_PRODUCT_CATEGORY(
'Bushing housing and upper spring seat',
'Bushing housing and upper spring seat',(#22883));
#22831=PRODUCT_RELATED_PRODUCT_CATEGORY(
'Bushing housing and upper spring seat (1)',
'Bushing housing and upper spring seat (1)',(#22884));
#22832=PRODUCT_RELATED_PRODUCT_CATEGORY(
'Bushing housing and upper spring seat (2)',
'Bushing housing and upper spring seat (2)',(#22885));
#22833=PRODUCT_RELATED_PRODUCT_CATEGORY(
'Bushing housing and upper spring seat (3)',
'Bushing housing and upper spring seat (3)',(#22886));
#22834=PRODUCT_RELATED_PRODUCT_CATEGORY('Armature','Armature',(#22887));
#22835=PRODUCT_RELATED_PRODUCT_CATEGORY(
'Linear Ball Bushing - 12 x 21 x 30 mm',
'Linear Ball Bushing - 12 x 21 x 30 mm',(#22888));
#22836=PRODUCT_RELATED_PRODUCT_CATEGORY('Steel sleeve','Steel sleeve',(#22889));
#22837=PRODUCT_RELATED_PRODUCT_CATEGORY('Ball retainer (plastic)',
'Ball retainer (plastic)',(#22890));
#22838=PRODUCT_RELATED_PRODUCT_CATEGORY('Cap Screw - M4x16',
'Cap Screw - M4x16',(#22891));
#22839=APPLICATION_PROTOCOL_DEFINITION('international standard',
'automotive_design',2009,#22840);
#22840=APPLICATION_CONTEXT(
'Core Data for Automotive Mechanical Design Process');
#22841=PRODUCT_CONTEXT('part definition',#22840,'mechanical');
#22842=PRODUCT('PAT-120','PAT-120',
'PAT-120',(#22841));
#22843=PRODUCT('Frame and installed return springs',
'Frame and installed return springs',
'Frame and installed return springs',(#22841));
#22844=PRODUCT('Base','Base','Base',(#22841));
#22845=PRODUCT('Foot strip','Foot strip','Foot strip',(#22841));
#22846=PRODUCT('Foot strip (1)','Foot strip (1)','Foot strip (1)',(#22841));
#22847=PRODUCT('Guide header','Guide header','Guide header',(#22841));
#22848=PRODUCT('Frame upright','Frame upright','Frame upright',(#22841));
#22849=PRODUCT('Frame upright (1)','Frame upright (1)','Frame upright (1)',(#22841));
#22850=PRODUCT('Lower guide bracket','Lower guide bracket',
'Lower guide bracket',(#22841));
#22851=PRODUCT('Upper guide bracket','Upper guide bracket',
'Upper guide bracket',(#22841));
#22852=PRODUCT('Lower spring seat','Lower spring seat',
'Lower spring seat',(#22841));
#22853=PRODUCT('Installed compression spring',
'Installed compression spring','Installed compression spring',(#22841));
#22854=PRODUCT('Lower guide bracket (1)','Lower guide bracket (1)',
'Lower guide bracket (1)',(#22841));
#22855=PRODUCT('Upper guide bracket (1)','Upper guide bracket (1)',
'Upper guide bracket (1)',(#22841));
#22856=PRODUCT('Lower spring seat (1)','Lower spring seat (1)',
'Lower spring seat (1)',(#22841));
#22857=PRODUCT('Installed compression spring (1)',
'Installed compression spring (1)','Installed compression spring (1)',(#22841));
#22858=PRODUCT('Lower guide bracket (2)','Lower guide bracket (2)',
'Lower guide bracket (2)',(#22841));
#22859=PRODUCT('Upper guide bracket (2)','Upper guide bracket (2)',
'Upper guide bracket (2)',(#22841));
#22860=PRODUCT('Lower spring seat (2)','Lower spring seat (2)',
'Lower spring seat (2)',(#22841));
#22861=PRODUCT('Installed compression spring (2)',
'Installed compression spring (2)','Installed compression spring (2)',(#22841));
#22862=PRODUCT('Lower guide bracket (3)','Lower guide bracket (3)',
'Lower guide bracket (3)',(#22841));
#22863=PRODUCT('Upper guide bracket (3)','Upper guide bracket (3)',
'Upper guide bracket (3)',(#22841));
#22864=PRODUCT('Lower spring seat (3)','Lower spring seat (3)',
'Lower spring seat (3)',(#22841));
#22865=PRODUCT('Installed compression spring (3)',
'Installed compression spring (3)','Installed compression spring (3)',(#22841));
#22866=PRODUCT('Exciter envelope','Exciter envelope','Exciter envelope',
(#22841));
#22867=PRODUCT('Exciter base flange','Exciter base flange',
'Exciter base flange',(#22841));
#22868=PRODUCT('Armature guide bush','Armature guide bush',
'Armature guide bush',(#22841));
#22869=PRODUCT('Lower stop post','Lower stop post','Lower stop post',(#22841));
#22870=PRODUCT('Stop bumper','Stop bumper','Stop bumper',(#22841));
#22871=PRODUCT('Upper stop post','Upper stop post','Upper stop post',(#22841));
#22872=PRODUCT('Stop bumper (1)','Stop bumper (1)','Stop bumper (1)',(#22841));
#22873=PRODUCT('Lower stop post (1)','Lower stop post (1)',
'Lower stop post (1)',(#22841));
#22874=PRODUCT('Stop bumper (2)','Stop bumper (2)','Stop bumper (2)',(#22841));
#22875=PRODUCT('Upper stop post (1)','Upper stop post (1)',
'Upper stop post (1)',(#22841));
#22876=PRODUCT('Stop bumper (3)','Stop bumper (3)','Stop bumper (3)',(#22841));
#22877=PRODUCT('Precision Shaft - 12 mm Diameter, 300 mm Long',
'Precision Shaft - 12 mm Diameter, 300 mm Long',
'Precision Shaft - 12 mm Diameter, 300 mm Long',(#22841));
#22878=PRODUCT('Shaft Support - 12 mm Bore',
'Shaft Support - 12 mm Bore','Shaft Support - 12 mm Bore',(#22841));
#22879=PRODUCT('M5x14 Cap Screw','M5x14 Cap Screw','M5x14 Cap Screw',(#22841));
#22880=PRODUCT('Cap Screw - M5x20','Cap Screw - M5x20',
'Cap Screw - M5x20',(#22841));
#22881=PRODUCT('Guided table and armature','Guided table and armature',
'Guided table and armature',(#22841));
#22882=PRODUCT('Table','Table','Table',(#22841));
#22883=PRODUCT('Bushing housing and upper spring seat',
'Bushing housing and upper spring seat',
'Bushing housing and upper spring seat',(#22841));
#22884=PRODUCT('Bushing housing and upper spring seat (1)',
'Bushing housing and upper spring seat (1)',
'Bushing housing and upper spring seat (1)',(#22841));
#22885=PRODUCT('Bushing housing and upper spring seat (2)',
'Bushing housing and upper spring seat (2)',
'Bushing housing and upper spring seat (2)',(#22841));
#22886=PRODUCT('Bushing housing and upper spring seat (3)',
'Bushing housing and upper spring seat (3)',
'Bushing housing and upper spring seat (3)',(#22841));
#22887=PRODUCT('Armature','Armature','Armature',(#22841));
#22888=PRODUCT('Linear Ball Bushing - 12 x 21 x 30 mm',
'Linear Ball Bushing - 12 x 21 x 30 mm',
'Linear Ball Bushing - 12 x 21 x 30 mm',(#22841));
#22889=PRODUCT('Steel sleeve','Steel sleeve','Steel sleeve',(#22841));
#22890=PRODUCT('Ball retainer (plastic)','Ball retainer (plastic)',
'Ball retainer (plastic)',(#22841));
#22891=PRODUCT('Cap Screw - M4x16','Cap Screw - M4x16',
'Cap Screw - M4x16',(#22841));
#22892=PRESENTATION_STYLE_ASSIGNMENT((#22898));
#22893=PRESENTATION_STYLE_ASSIGNMENT((#22899));
#22894=PRESENTATION_STYLE_ASSIGNMENT((#22900));
#22895=PRESENTATION_STYLE_ASSIGNMENT((#22901));
#22896=PRESENTATION_STYLE_ASSIGNMENT((#22902));
#22897=PRESENTATION_STYLE_ASSIGNMENT((#22903));
#22898=SURFACE_STYLE_USAGE(.BOTH.,#22904);
#22899=SURFACE_STYLE_USAGE(.BOTH.,#22905);
#22900=SURFACE_STYLE_USAGE(.BOTH.,#22906);
#22901=SURFACE_STYLE_USAGE(.BOTH.,#22907);
#22902=SURFACE_STYLE_USAGE(.BOTH.,#22908);
#22903=SURFACE_STYLE_USAGE(.BOTH.,#22909);
#22904=SURFACE_SIDE_STYLE('',(#22910));
#22905=SURFACE_SIDE_STYLE('',(#22911));
#22906=SURFACE_SIDE_STYLE('',(#22912));
#22907=SURFACE_SIDE_STYLE('',(#22913));
#22908=SURFACE_SIDE_STYLE('',(#22914));
#22909=SURFACE_SIDE_STYLE('',(#22915));
#22910=SURFACE_STYLE_FILL_AREA(#22916);
#22911=SURFACE_STYLE_FILL_AREA(#22917);
#22912=SURFACE_STYLE_FILL_AREA(#22918);
#22913=SURFACE_STYLE_FILL_AREA(#22919);
#22914=SURFACE_STYLE_FILL_AREA(#22920);
#22915=SURFACE_STYLE_FILL_AREA(#22921);
#22916=FILL_AREA_STYLE('Steel - Satin',(#22922));
#22917=FILL_AREA_STYLE('CAD Library Painted - Deep blue',(#22923));
#22918=FILL_AREA_STYLE('CAD Library Painted - Engineering blue',(#22924));
#22919=FILL_AREA_STYLE('CAD Library Painted - Steel gray',(#22925));
#22920=FILL_AREA_STYLE('CAD Library Painted - Graphite',(#22926));
#22921=FILL_AREA_STYLE('CAD Library Painted - Light blue',(#22927));
#22922=FILL_AREA_STYLE_COLOUR('Steel - Satin',#22928);
#22923=FILL_AREA_STYLE_COLOUR('CAD Library Painted - Deep blue',#22929);
#22924=FILL_AREA_STYLE_COLOUR('CAD Library Painted - Engineering blue',
#22930);
#22925=FILL_AREA_STYLE_COLOUR('CAD Library Painted - Steel gray',#22931);
#22926=FILL_AREA_STYLE_COLOUR('CAD Library Painted - Graphite',#22932);
#22927=FILL_AREA_STYLE_COLOUR('CAD Library Painted - Light blue',#22933);
#22928=COLOUR_RGB('Steel - Satin',0.627450980392157,0.627450980392157,0.627450980392157);
#22929=COLOUR_RGB('CAD Library Painted - Deep blue',0.0784313725490196,
0.203921568627451,0.349019607843137);
#22930=COLOUR_RGB('CAD Library Painted - Engineering blue',0.12156862745098,
0.356862745098039,0.6);
#22931=COLOUR_RGB('CAD Library Painted - Steel gray',0.592156862745098,
0.631372549019608,0.67843137254902);
#22932=COLOUR_RGB('CAD Library Painted - Graphite',0.168627450980392,0.192156862745098,
0.231372549019608);
#22933=COLOUR_RGB('CAD Library Painted - Light blue',0.286274509803922,
0.552941176470588,0.780392156862745);
#22934=COLOUR_RGB('Dark Blue',0.08,0.2,0.34);
#22935=FILL_AREA_STYLE_COLOUR('',#22934);
#22936=FILL_AREA_STYLE('',(#22935));
#22937=SURFACE_STYLE_FILL_AREA(#22936);
#22938=SURFACE_SIDE_STYLE('',(#22937));
#22939=SURFACE_STYLE_USAGE(.BOTH.,#22938);
#22940=PRESENTATION_STYLE_ASSIGNMENT((#22939));
#22941=COLOUR_RGB('Light Blue',0.38,0.62,0.78);
#22942=FILL_AREA_STYLE_COLOUR('',#22941);
#22943=FILL_AREA_STYLE('',(#22942));
#22944=SURFACE_STYLE_FILL_AREA(#22943);
#22945=SURFACE_SIDE_STYLE('',(#22944));
#22946=SURFACE_STYLE_USAGE(.BOTH.,#22945);
#22947=PRESENTATION_STYLE_ASSIGNMENT((#22946));
#22948=COLOUR_RGB('Sky Blue',0.24,0.69,0.87);
#22949=FILL_AREA_STYLE_COLOUR('',#22948);
#22950=FILL_AREA_STYLE('',(#22949));
#22951=SURFACE_STYLE_FILL_AREA(#22950);
#22952=SURFACE_SIDE_STYLE('',(#22951));
#22953=SURFACE_STYLE_USAGE(.BOTH.,#22952);
#22954=PRESENTATION_STYLE_ASSIGNMENT((#22953));
#22955=COLOUR_RGB('Grey',0.48,0.52,0.57);
#22956=FILL_AREA_STYLE_COLOUR('',#22955);
#22957=FILL_AREA_STYLE('',(#22956));
#22958=SURFACE_STYLE_FILL_AREA(#22957);
#22959=SURFACE_SIDE_STYLE('',(#22958));
#22960=SURFACE_STYLE_USAGE(.BOTH.,#22959);
#22961=PRESENTATION_STYLE_ASSIGNMENT((#22960));
#22962=COLOUR_RGB('Black',0.12,0.14,0.17);
#22963=FILL_AREA_STYLE_COLOUR('',#22962);
#22964=FILL_AREA_STYLE('',(#22963));
#22965=SURFACE_STYLE_FILL_AREA(#22964);
#22966=SURFACE_SIDE_STYLE('',(#22965));
#22967=SURFACE_STYLE_USAGE(.BOTH.,#22966);
#22968=PRESENTATION_STYLE_ASSIGNMENT((#22967));
#22969=COLOUR_RGB('Off White',0.89,0.88,0.83);
#22970=FILL_AREA_STYLE_COLOUR('',#22969);
#22971=FILL_AREA_STYLE('',(#22970));
#22972=SURFACE_STYLE_FILL_AREA(#22971);
#22973=SURFACE_SIDE_STYLE('',(#22972));
#22974=SURFACE_STYLE_USAGE(.BOTH.,#22973);
#22975=PRESENTATION_STYLE_ASSIGNMENT((#22974));
ENDSEC;
END-ISO-10303-21;
